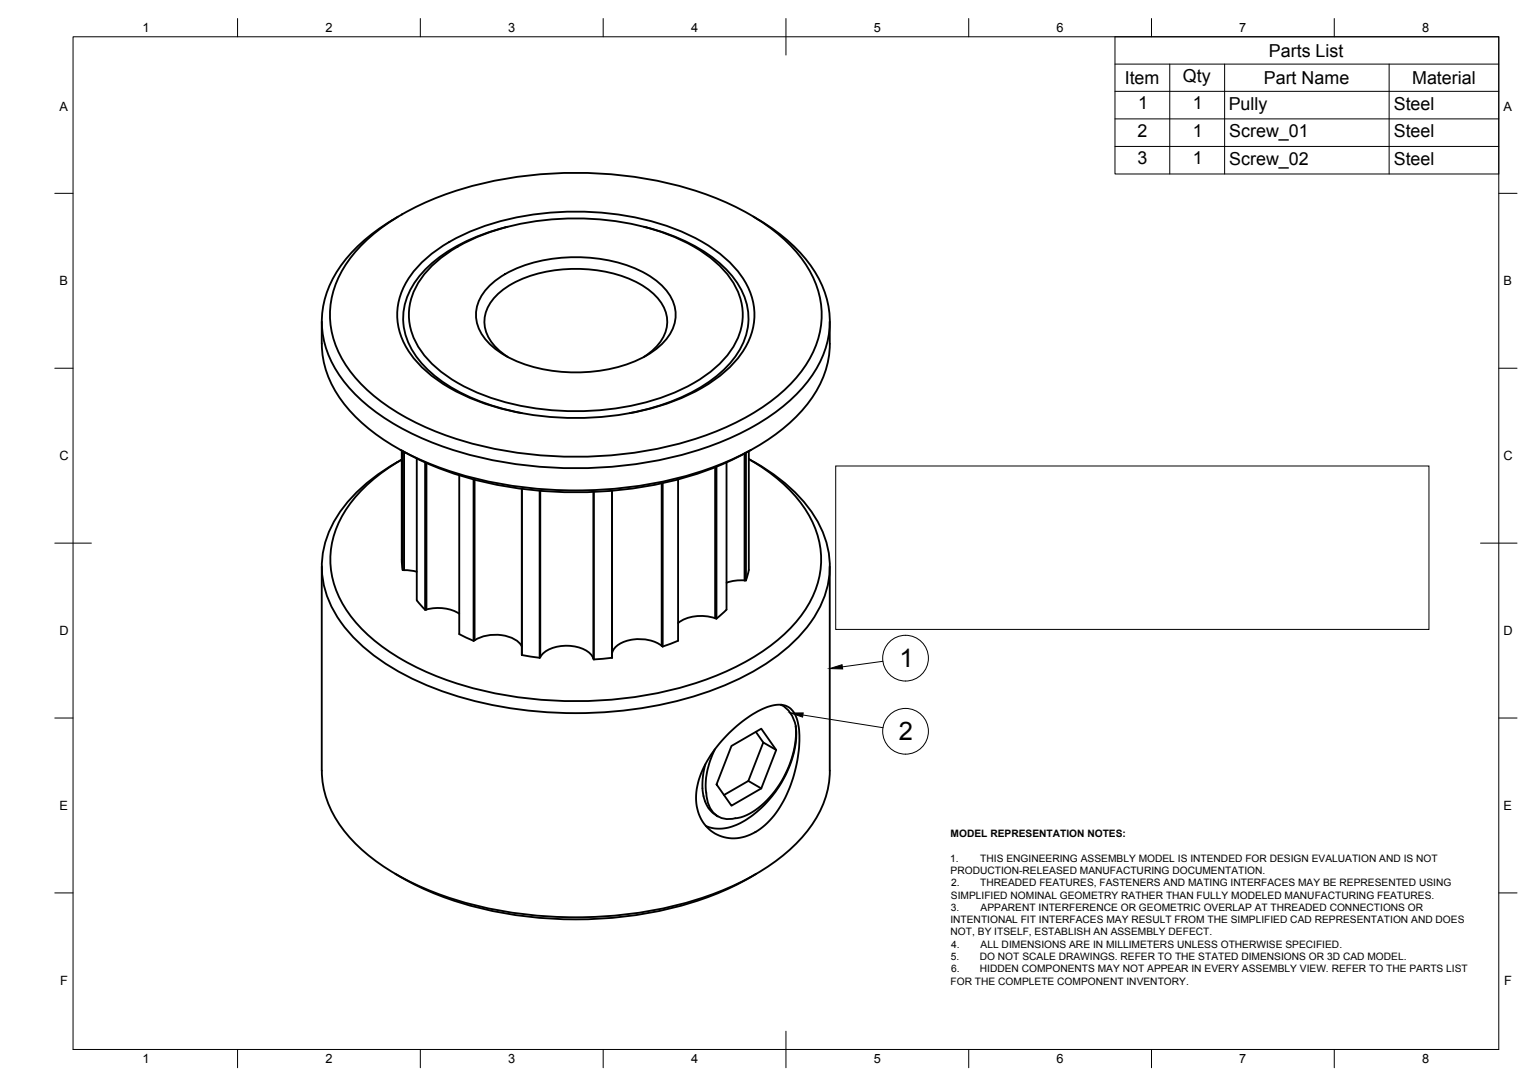
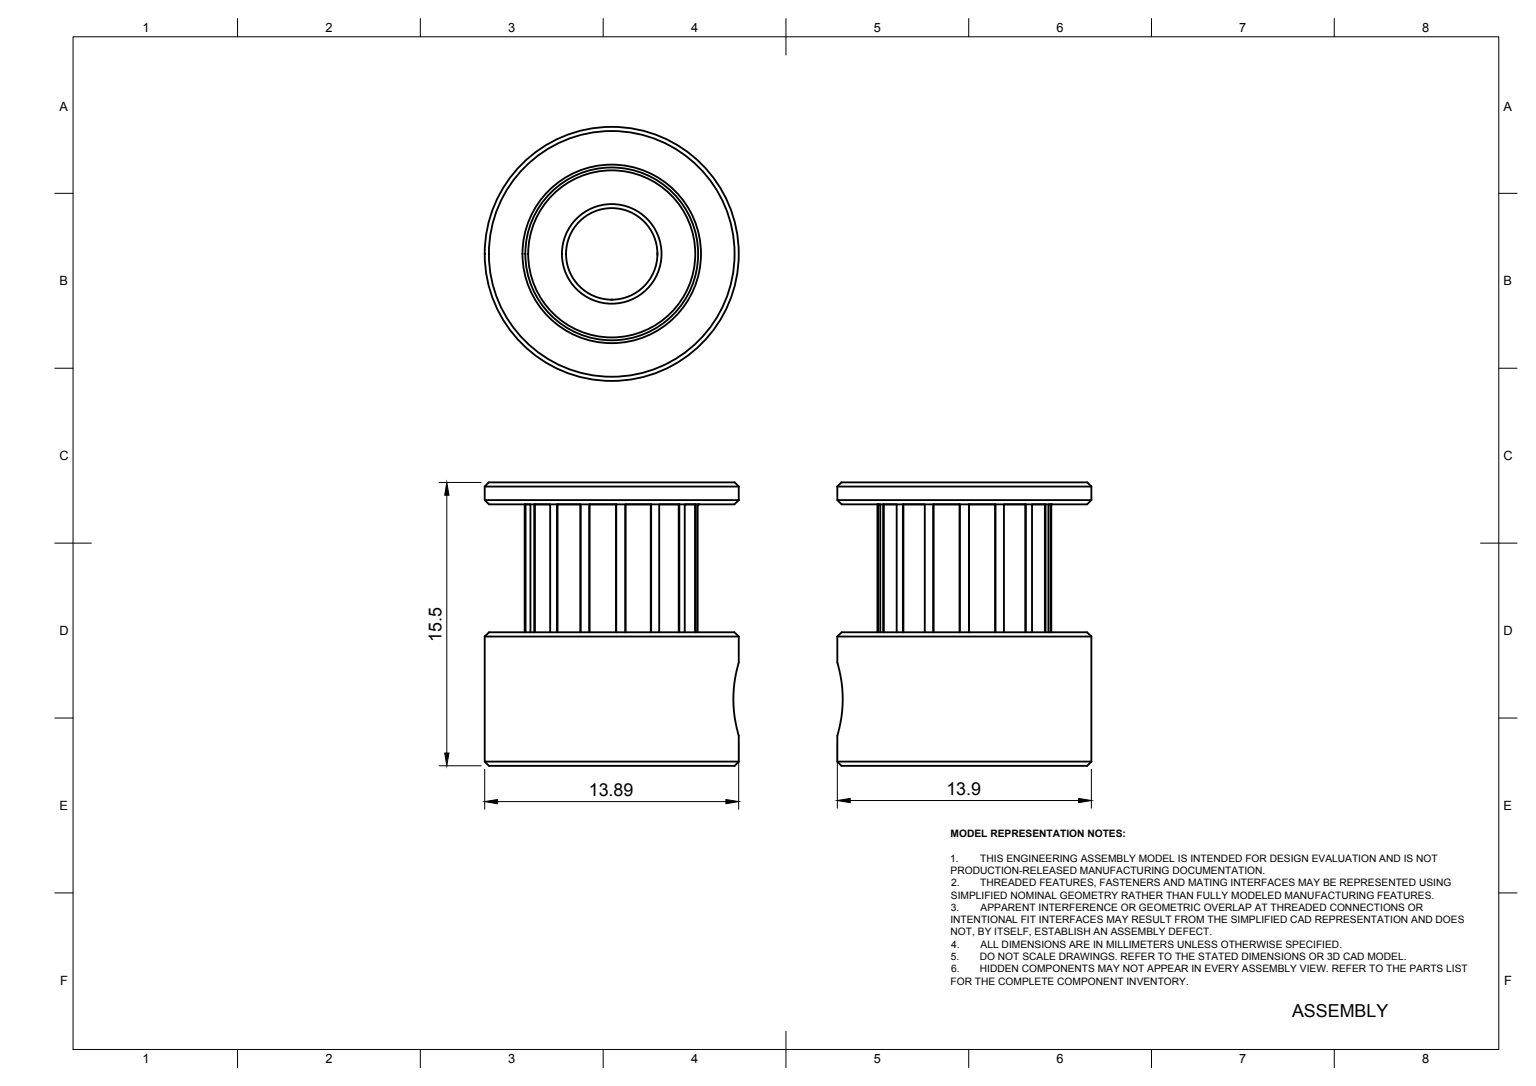
ISO-10303-21;
HEADER;
/* Generated by software containing ST-Developer
 * from STEP Tools, Inc. (www.steptools.com) 
 */

FILE_DESCRIPTION(
/* description */ (''),
/* implementation_level */ '2;1');

FILE_NAME(
/* name */ 'BR-253',
/* time_stamp */ '2026-10-05T21:25:27-07:00',
/* author */ (''),
/* organization */ (''),
/* preprocessor_version */ 'ST-DEVELOPER v20.2',
/* originating_system */ 'Autodesk Translation Framework v15.15.0.0',
/* authorisation */ '');

FILE_SCHEMA (('AUTOMOTIVE_DESIGN { 1 0 10303 214 3 1 1 }'));
ENDSEC;

DATA;
#10=MECHANICAL_DESIGN_GEOMETRIC_PRESENTATION_REPRESENTATION('',(#33,#34,
#35),#12118);
#11=ITEM_DEFINED_TRANSFORMATION($,$,#2444,#2723);
#12=ITEM_DEFINED_TRANSFORMATION($,$,#2667,#2724);
#13=ITEM_DEFINED_TRANSFORMATION($,$,#2695,#2725);
#14=(
REPRESENTATION_RELATIONSHIP($,$,#12135,#12134)
REPRESENTATION_RELATIONSHIP_WITH_TRANSFORMATION(#11)
SHAPE_REPRESENTATION_RELATIONSHIP()
);
#15=(
REPRESENTATION_RELATIONSHIP($,$,#12136,#12134)
REPRESENTATION_RELATIONSHIP_WITH_TRANSFORMATION(#12)
SHAPE_REPRESENTATION_RELATIONSHIP()
);
#16=(
REPRESENTATION_RELATIONSHIP($,$,#12137,#12134)
REPRESENTATION_RELATIONSHIP_WITH_TRANSFORMATION(#13)
SHAPE_REPRESENTATION_RELATIONSHIP()
);
#17=CONTEXT_DEPENDENT_SHAPE_REPRESENTATION(#14,#12131);
#18=CONTEXT_DEPENDENT_SHAPE_REPRESENTATION(#15,#12132);
#19=CONTEXT_DEPENDENT_SHAPE_REPRESENTATION(#16,#12133);
#20=NEXT_ASSEMBLY_USAGE_OCCURRENCE('Pully:1','Pully:1','Pully:1',#12139,
#12140,'Pully:1');
#21=NEXT_ASSEMBLY_USAGE_OCCURRENCE('Screw_01:1','Screw_01:1',
'Screw_01:1',#12139,#12141,'Screw_01:1');
#22=NEXT_ASSEMBLY_USAGE_OCCURRENCE('Screw_02:1','Screw_02:1',
'Screw_02:1',#12139,#12142,'Screw_02:1');
#23=B_SPLINE_SURFACE_WITH_KNOTS('',3,3,((#7351,#7352,#7353,#7354,#7355,
#7356,#7357,#7358,#7359,#7360,#7361,#7362,#7363,#7364,#7365,#7366,#7367,
#7368,#7369,#7370,#7371,#7372,#7373,#7374,#7375,#7376,#7377,#7378,#7379,
#7380,#7381,#7382,#7383,#7384,#7385,#7386,#7387,#7388,#7389,#7390,#7391,
#7392),(#7393,#7394,#7395,#7396,#7397,#7398,#7399,#7400,#7401,#7402,#7403,
#7404,#7405,#7406,#7407,#7408,#7409,#7410,#7411,#7412,#7413,#7414,#7415,
#7416,#7417,#7418,#7419,#7420,#7421,#7422,#7423,#7424,#7425,#7426,#7427,
#7428,#7429,#7430,#7431,#7432,#7433,#7434),(#7435,#7436,#7437,#7438,#7439,
#7440,#7441,#7442,#7443,#7444,#7445,#7446,#7447,#7448,#7449,#7450,#7451,
#7452,#7453,#7454,#7455,#7456,#7457,#7458,#7459,#7460,#7461,#7462,#7463,
#7464,#7465,#7466,#7467,#7468,#7469,#7470,#7471,#7472,#7473,#7474,#7475,
#7476),(#7477,#7478,#7479,#7480,#7481,#7482,#7483,#7484,#7485,#7486,#7487,
#7488,#7489,#7490,#7491,#7492,#7493,#7494,#7495,#7496,#7497,#7498,#7499,
#7500,#7501,#7502,#7503,#7504,#7505,#7506,#7507,#7508,#7509,#7510,#7511,
#7512,#7513,#7514,#7515,#7516,#7517,#7518)),.UNSPECIFIED.,.F.,.F.,.F.,(4,
4),(4,1,1,1,1,1,1,1,1,1,1,1,1,1,1,1,1,1,1,1,1,1,1,1,1,1,1,1,1,1,1,1,1,1,
1,1,1,1,1,4),(-0.000255169100126038,0.0463066876673496),(8.31044341387851,
9.3071677964662,10.3037486701926,11.300329543919,12.2969104176454,13.2934912913718,
14.2900721650982,15.2866530388247,16.2832339125511,17.2798147862775,18.2763956600039,
19.2729765337303,20.2695574074567,21.2661382811831,22.2627191549095,23.2593000286359,
24.2558809023623,25.2524617760888,26.2490426498152,27.2456235235416,28.242204397268,
29.2387852709944,30.2353661447208,31.2319470184472,32.2285278921736,33.2251087659,
34.2216896396264,35.2182705133528,36.2148513870793,37.2114322608057,38.2080131345321,
39.2045940082585,40.2011748819849,41.1977557557113,42.1943366294377,43.1909175031641,
44.1874983768905,45.1840792506169,46.1806601243433,47.1772409980698),
 .UNSPECIFIED.);
#24=B_SPLINE_SURFACE_WITH_KNOTS('',3,3,((#7695,#7696,#7697,#7698,#7699,
#7700,#7701,#7702,#7703,#7704,#7705,#7706,#7707,#7708,#7709,#7710,#7711,
#7712,#7713,#7714,#7715,#7716,#7717,#7718,#7719,#7720,#7721,#7722,#7723,
#7724,#7725,#7726,#7727,#7728,#7729,#7730,#7731,#7732,#7733,#7734,#7735,
#7736),(#7737,#7738,#7739,#7740,#7741,#7742,#7743,#7744,#7745,#7746,#7747,
#7748,#7749,#7750,#7751,#7752,#7753,#7754,#7755,#7756,#7757,#7758,#7759,
#7760,#7761,#7762,#7763,#7764,#7765,#7766,#7767,#7768,#7769,#7770,#7771,
#7772,#7773,#7774,#7775,#7776,#7777,#7778),(#7779,#7780,#7781,#7782,#7783,
#7784,#7785,#7786,#7787,#7788,#7789,#7790,#7791,#7792,#7793,#7794,#7795,
#7796,#7797,#7798,#7799,#7800,#7801,#7802,#7803,#7804,#7805,#7806,#7807,
#7808,#7809,#7810,#7811,#7812,#7813,#7814,#7815,#7816,#7817,#7818,#7819,
#7820),(#7821,#7822,#7823,#7824,#7825,#7826,#7827,#7828,#7829,#7830,#7831,
#7832,#7833,#7834,#7835,#7836,#7837,#7838,#7839,#7840,#7841,#7842,#7843,
#7844,#7845,#7846,#7847,#7848,#7849,#7850,#7851,#7852,#7853,#7854,#7855,
#7856,#7857,#7858,#7859,#7860,#7861,#7862)),.UNSPECIFIED.,.F.,.F.,.F.,(4,
4),(4,1,1,1,1,1,1,1,1,1,1,1,1,1,1,1,1,1,1,1,1,1,1,1,1,1,1,1,1,1,1,1,1,1,
1,1,1,1,1,4),(-0.000278939256451679,0.0463345324070479),(11.6151018031581,
12.6120023928371,13.6085832665635,14.6051641402899,15.6017450140163,16.5983258877427,
17.5949067614691,18.5914876351955,19.5880685089219,20.5846493826483,21.5812302563748,
22.5778111301012,23.5743920038276,24.570972877554,25.5675537512804,26.5641346250068,
27.5607154987332,28.5572963724596,29.553877246186,30.5504581199124,31.5470389936388,
32.5436198673653,33.5402007410917,34.5367816148181,35.5333624885445,36.5299433622709,
37.5265242359973,38.5231051097237,39.5196859834501,40.5162668571765,41.5128477309029,
42.5094286046293,43.5060094783558,44.5025903520822,45.4991712258086,46.495752099535,
47.4923329732614,48.4889138469878,49.4854947207142,50.4820755944406),
 .UNSPECIFIED.);
#25=B_SPLINE_SURFACE_WITH_KNOTS('',3,3,((#11379,#11380,#11381,#11382,#11383,
#11384,#11385,#11386,#11387,#11388,#11389,#11390,#11391,#11392,#11393,#11394,
#11395,#11396,#11397,#11398,#11399,#11400,#11401,#11402,#11403,#11404,#11405,
#11406,#11407,#11408,#11409,#11410,#11411,#11412,#11413,#11414,#11415,#11416,
#11417,#11418,#11419,#11420),(#11421,#11422,#11423,#11424,#11425,#11426,
#11427,#11428,#11429,#11430,#11431,#11432,#11433,#11434,#11435,#11436,#11437,
#11438,#11439,#11440,#11441,#11442,#11443,#11444,#11445,#11446,#11447,#11448,
#11449,#11450,#11451,#11452,#11453,#11454,#11455,#11456,#11457,#11458,#11459,
#11460,#11461,#11462),(#11463,#11464,#11465,#11466,#11467,#11468,#11469,
#11470,#11471,#11472,#11473,#11474,#11475,#11476,#11477,#11478,#11479,#11480,
#11481,#11482,#11483,#11484,#11485,#11486,#11487,#11488,#11489,#11490,#11491,
#11492,#11493,#11494,#11495,#11496,#11497,#11498,#11499,#11500,#11501,#11502,
#11503,#11504),(#11505,#11506,#11507,#11508,#11509,#11510,#11511,#11512,
#11513,#11514,#11515,#11516,#11517,#11518,#11519,#11520,#11521,#11522,#11523,
#11524,#11525,#11526,#11527,#11528,#11529,#11530,#11531,#11532,#11533,#11534,
#11535,#11536,#11537,#11538,#11539,#11540,#11541,#11542,#11543,#11544,#11545,
#11546)),.UNSPECIFIED.,.F.,.F.,.F.,(4,4),(4,1,1,1,1,1,1,1,1,1,1,1,1,1,1,
1,1,1,1,1,1,1,1,1,1,1,1,1,1,1,1,1,1,1,1,1,1,1,1,4),(-0.000255169100126093,
0.0463066876673497),(8.31044341387851,9.3071677964662,10.3037486701926,
11.300329543919,12.2969104176454,13.2934912913718,14.2900721650982,15.2866530388247,
16.2832339125511,17.2798147862775,18.2763956600039,19.2729765337303,20.2695574074567,
21.2661382811831,22.2627191549095,23.2593000286359,24.2558809023623,25.2524617760888,
26.2490426498152,27.2456235235416,28.242204397268,29.2387852709944,30.2353661447208,
31.2319470184472,32.2285278921736,33.2251087659,34.2216896396264,35.2182705133528,
36.2148513870793,37.2114322608057,38.2080131345321,39.2045940082585,40.2011748819849,
41.1977557557113,42.1943366294377,43.1909175031641,44.1874983768905,45.1840792506169,
46.1806601243433,47.1772409980698),.UNSPECIFIED.);
#26=B_SPLINE_SURFACE_WITH_KNOTS('',3,3,((#11723,#11724,#11725,#11726,#11727,
#11728,#11729,#11730,#11731,#11732,#11733,#11734,#11735,#11736,#11737,#11738,
#11739,#11740,#11741,#11742,#11743,#11744,#11745,#11746,#11747,#11748,#11749,
#11750,#11751,#11752,#11753,#11754,#11755,#11756,#11757,#11758,#11759,#11760,
#11761,#11762,#11763,#11764),(#11765,#11766,#11767,#11768,#11769,#11770,
#11771,#11772,#11773,#11774,#11775,#11776,#11777,#11778,#11779,#11780,#11781,
#11782,#11783,#11784,#11785,#11786,#11787,#11788,#11789,#11790,#11791,#11792,
#11793,#11794,#11795,#11796,#11797,#11798,#11799,#11800,#11801,#11802,#11803,
#11804,#11805,#11806),(#11807,#11808,#11809,#11810,#11811,#11812,#11813,
#11814,#11815,#11816,#11817,#11818,#11819,#11820,#11821,#11822,#11823,#11824,
#11825,#11826,#11827,#11828,#11829,#11830,#11831,#11832,#11833,#11834,#11835,
#11836,#11837,#11838,#11839,#11840,#11841,#11842,#11843,#11844,#11845,#11846,
#11847,#11848),(#11849,#11850,#11851,#11852,#11853,#11854,#11855,#11856,
#11857,#11858,#11859,#11860,#11861,#11862,#11863,#11864,#11865,#11866,#11867,
#11868,#11869,#11870,#11871,#11872,#11873,#11874,#11875,#11876,#11877,#11878,
#11879,#11880,#11881,#11882,#11883,#11884,#11885,#11886,#11887,#11888,#11889,
#11890)),.UNSPECIFIED.,.F.,.F.,.F.,(4,4),(4,1,1,1,1,1,1,1,1,1,1,1,1,1,1,
1,1,1,1,1,1,1,1,1,1,1,1,1,1,1,1,1,1,1,1,1,1,1,1,4),(-0.000278939256451637,
0.046334532407048),(11.6151018031581,12.6120023928371,13.6085832665635,
14.6051641402899,15.6017450140163,16.5983258877427,17.5949067614691,18.5914876351955,
19.5880685089219,20.5846493826483,21.5812302563748,22.5778111301012,23.5743920038276,
24.570972877554,25.5675537512804,26.5641346250068,27.5607154987332,28.5572963724596,
29.553877246186,30.5504581199124,31.5470389936388,32.5436198673653,33.5402007410917,
34.5367816148181,35.5333624885445,36.5299433622709,37.5265242359973,38.5231051097237,
39.5196859834501,40.5162668571765,41.5128477309029,42.5094286046293,43.5060094783558,
44.5025903520822,45.4991712258086,46.495752099535,47.4923329732614,48.4889138469878,
49.4854947207142,50.4820755944406),.UNSPECIFIED.);
#27=SHAPE_REPRESENTATION_RELATIONSHIP('SRR','None',#12135,#30);
#28=SHAPE_REPRESENTATION_RELATIONSHIP('SRR','None',#12136,#31);
#29=SHAPE_REPRESENTATION_RELATIONSHIP('SRR','None',#12137,#32);
#30=ADVANCED_BREP_SHAPE_REPRESENTATION('',(#36),#12115);
#31=ADVANCED_BREP_SHAPE_REPRESENTATION('',(#37),#12116);
#32=ADVANCED_BREP_SHAPE_REPRESENTATION('',(#38),#12117);
#33=STYLED_ITEM('',(#12159),#36);
#34=STYLED_ITEM('',(#12159),#37);
#35=STYLED_ITEM('',(#12159),#38);
#36=MANIFOLD_SOLID_BREP('Body1',#2406);
#37=MANIFOLD_SOLID_BREP('Body1',#2407);
#38=MANIFOLD_SOLID_BREP('Body1',#2408);
#39=CONICAL_SURFACE('',#2637,6.82923606324244,0.788206310939685);
#40=CONICAL_SURFACE('',#2641,6.83201065632366,0.782590015855212);
#41=CONICAL_SURFACE('',#2645,4.80296382139185,0.926815431707518);
#42=CONICAL_SURFACE('',#2647,4.64521779108966,0.920500215637548);
#43=CONICAL_SURFACE('',#2651,2.61128051468949,0.789543103695558);
#44=CONICAL_SURFACE('',#2652,2.61559010295572,0.781253223099339);
#45=CONICAL_SURFACE('',#2656,4.64520588040018,0.911866720012535);
#46=CONICAL_SURFACE('',#2658,4.80503122320831,0.931803832862888);
#47=CONICAL_SURFACE('',#2662,6.83593993841137,0.77406839497658);
#48=CONICAL_SURFACE('',#2666,6.82905809599587,0.796727931818318);
#49=FACE_BOUND('',#442,.T.);
#50=FACE_BOUND('',#444,.T.);
#51=FACE_BOUND('',#447,.T.);
#52=FACE_BOUND('',#450,.T.);
#53=FACE_BOUND('',#454,.T.);
#54=FACE_BOUND('',#458,.T.);
#55=FACE_BOUND('',#462,.T.);
#56=FACE_BOUND('',#483,.T.);
#57=FACE_BOUND('',#509,.T.);
#58=PLANE('',#2453);
#59=PLANE('',#2464);
#60=PLANE('',#2475);
#61=PLANE('',#2486);
#62=PLANE('',#2497);
#63=PLANE('',#2508);
#64=PLANE('',#2519);
#65=PLANE('',#2530);
#66=PLANE('',#2541);
#67=PLANE('',#2552);
#68=PLANE('',#2563);
#69=PLANE('',#2574);
#70=PLANE('',#2585);
#71=PLANE('',#2596);
#72=PLANE('',#2626);
#73=PLANE('',#2633);
#74=PLANE('',#2635);
#75=PLANE('',#2643);
#76=PLANE('',#2649);
#77=PLANE('',#2654);
#78=PLANE('',#2660);
#79=PLANE('',#2686);
#80=PLANE('',#2687);
#81=PLANE('',#2688);
#82=PLANE('',#2689);
#83=PLANE('',#2690);
#84=PLANE('',#2691);
#85=PLANE('',#2692);
#86=PLANE('',#2693);
#87=PLANE('',#2694);
#88=PLANE('',#2714);
#89=PLANE('',#2715);
#90=PLANE('',#2716);
#91=PLANE('',#2717);
#92=PLANE('',#2718);
#93=PLANE('',#2719);
#94=PLANE('',#2720);
#95=PLANE('',#2721);
#96=PLANE('',#2722);
#97=CIRCLE('',#2447,2.50080065552765);
#98=CIRCLE('',#2448,2.50080065552765);
#99=CIRCLE('',#2451,0.124032861755453);
#100=CIRCLE('',#2452,0.124032861755453);
#101=CIRCLE('',#2454,4.75930776765241);
#102=CIRCLE('',#2455,0.749041401963156);
#103=CIRCLE('',#2456,0.124032861755453);
#104=CIRCLE('',#2458,0.749041401963156);
#105=CIRCLE('',#2460,0.124032861755453);
#106=CIRCLE('',#2462,0.124032861755453);
#107=CIRCLE('',#2463,0.124032861755453);
#108=CIRCLE('',#2465,4.75930776765241);
#109=CIRCLE('',#2466,0.749041401963156);
#110=CIRCLE('',#2467,0.124032861755453);
#111=CIRCLE('',#2469,0.749041401963156);
#112=CIRCLE('',#2471,0.124032861755453);
#113=CIRCLE('',#2473,0.124032861755453);
#114=CIRCLE('',#2474,0.124032861755453);
#115=CIRCLE('',#2476,4.75930776765241);
#116=CIRCLE('',#2477,0.749041401963155);
#117=CIRCLE('',#2478,0.124032861755453);
#118=CIRCLE('',#2480,0.749041401963155);
#119=CIRCLE('',#2482,0.124032861755453);
#120=CIRCLE('',#2484,0.124032861755453);
#121=CIRCLE('',#2485,0.124032861755453);
#122=CIRCLE('',#2487,4.75930776765241);
#123=CIRCLE('',#2488,0.749041401963156);
#124=CIRCLE('',#2489,0.124032861755453);
#125=CIRCLE('',#2491,0.749041401963156);
#126=CIRCLE('',#2493,0.124032861755453);
#127=CIRCLE('',#2495,0.124032861755453);
#128=CIRCLE('',#2496,0.124032861755453);
#129=CIRCLE('',#2498,4.75930776765241);
#130=CIRCLE('',#2499,0.749041401963155);
#131=CIRCLE('',#2500,0.124032861755453);
#132=CIRCLE('',#2502,0.749041401963155);
#133=CIRCLE('',#2504,0.124032861755453);
#134=CIRCLE('',#2506,0.124032861755453);
#135=CIRCLE('',#2507,0.124032861755453);
#136=CIRCLE('',#2509,4.75930776765241);
#137=CIRCLE('',#2510,0.749041401963156);
#138=CIRCLE('',#2511,0.124032861755453);
#139=CIRCLE('',#2513,0.749041401963156);
#140=CIRCLE('',#2515,0.124032861755453);
#141=CIRCLE('',#2517,0.124032861755453);
#142=CIRCLE('',#2518,0.124032861755453);
#143=CIRCLE('',#2520,4.75930776765241);
#144=CIRCLE('',#2521,0.749041401963155);
#145=CIRCLE('',#2522,0.124032861755453);
#146=CIRCLE('',#2524,0.749041401963155);
#147=CIRCLE('',#2526,0.124032861755453);
#148=CIRCLE('',#2528,0.124032861755453);
#149=CIRCLE('',#2529,0.124032861755453);
#150=CIRCLE('',#2531,4.75930776765241);
#151=CIRCLE('',#2532,0.749041401963156);
#152=CIRCLE('',#2533,0.124032861755453);
#153=CIRCLE('',#2535,0.749041401963156);
#154=CIRCLE('',#2537,0.124032861755453);
#155=CIRCLE('',#2539,0.124032861755453);
#156=CIRCLE('',#2540,0.124032861755453);
#157=CIRCLE('',#2542,4.75930776765241);
#158=CIRCLE('',#2543,0.749041401963155);
#159=CIRCLE('',#2544,0.124032861755453);
#160=CIRCLE('',#2546,0.749041401963155);
#161=CIRCLE('',#2548,0.124032861755453);
#162=CIRCLE('',#2550,0.124032861755453);
#163=CIRCLE('',#2551,0.124032861755453);
#164=CIRCLE('',#2553,4.75930776765241);
#165=CIRCLE('',#2554,0.749041401963156);
#166=CIRCLE('',#2555,0.124032861755453);
#167=CIRCLE('',#2557,0.749041401963156);
#168=CIRCLE('',#2559,0.124032861755453);
#169=CIRCLE('',#2561,0.124032861755453);
#170=CIRCLE('',#2562,0.124032861755453);
#171=CIRCLE('',#2564,4.75930776765241);
#172=CIRCLE('',#2565,0.749041401963156);
#173=CIRCLE('',#2566,0.124032861755453);
#174=CIRCLE('',#2568,0.749041401963156);
#175=CIRCLE('',#2570,0.124032861755453);
#176=CIRCLE('',#2572,0.124032861755453);
#177=CIRCLE('',#2573,0.124032861755453);
#178=CIRCLE('',#2575,4.75930776765241);
#179=CIRCLE('',#2576,0.749041401963155);
#180=CIRCLE('',#2577,0.124032861755453);
#181=CIRCLE('',#2579,0.749041401963155);
#182=CIRCLE('',#2581,0.124032861755453);
#183=CIRCLE('',#2583,0.124032861755453);
#184=CIRCLE('',#2584,0.124032861755453);
#185=CIRCLE('',#2586,4.75930776765241);
#186=CIRCLE('',#2587,0.749041401963156);
#187=CIRCLE('',#2588,0.124032861755453);
#188=CIRCLE('',#2590,0.749041401963156);
#189=CIRCLE('',#2592,0.124032861755453);
#190=CIRCLE('',#2594,0.124032861755453);
#191=CIRCLE('',#2595,0.124032861755453);
#192=CIRCLE('',#2597,4.75930776765241);
#193=CIRCLE('',#2598,0.749041401963155);
#194=CIRCLE('',#2599,0.124032861755453);
#195=CIRCLE('',#2601,0.749041401963155);
#196=CIRCLE('',#2603,0.124032861755453);
#197=CIRCLE('',#2605,4.75930776765241);
#198=CIRCLE('',#2606,4.75930776765241);
#199=CIRCLE('',#2607,4.75930776765241);
#200=CIRCLE('',#2608,4.75930776765241);
#201=CIRCLE('',#2609,4.75930776765241);
#202=CIRCLE('',#2610,4.75930776765241);
#203=CIRCLE('',#2611,4.75930776765241);
#204=CIRCLE('',#2612,4.75930776765241);
#205=CIRCLE('',#2613,4.75930776765241);
#206=CIRCLE('',#2614,4.75930776765241);
#207=CIRCLE('',#2615,4.75930776765241);
#208=CIRCLE('',#2616,4.75930776765241);
#209=CIRCLE('',#2617,4.75930776765241);
#210=CIRCLE('',#2618,4.75930776765241);
#211=CIRCLE('',#2619,4.75930776765241);
#212=CIRCLE('',#2620,4.75930776765241);
#213=CIRCLE('',#2621,4.75930776765241);
#214=CIRCLE('',#2622,4.75930776765241);
#215=CIRCLE('',#2624,0.124032861755453);
#216=CIRCLE('',#2625,0.124032861755453);
#217=CIRCLE('',#2627,0.749041401963155);
#218=CIRCLE('',#2628,0.124032861755453);
#219=CIRCLE('',#2630,0.749041401963155);
#220=CIRCLE('',#2632,0.124032861755453);
#221=CIRCLE('',#2634,6.71146155382814);
#222=CIRCLE('',#2636,6.71146155382814);
#223=CIRCLE('',#2638,6.94701057265674);
#224=CIRCLE('',#2640,6.94701057265674);
#225=CIRCLE('',#2642,6.71701073999059);
#226=CIRCLE('',#2644,4.88235460250674);
#227=CIRCLE('',#2646,4.72357304027696);
#228=CIRCLE('',#2648,4.56686254190236);
#229=CIRCLE('',#2650,2.72176037385134);
#230=CIRCLE('',#2653,2.7303795503838);
#231=CIRCLE('',#2655,4.56694754124435);
#232=CIRCLE('',#2657,4.72346421955602);
#233=CIRCLE('',#2659,4.8865982268606);
#234=CIRCLE('',#2661,6.72522523865914);
#235=CIRCLE('',#2663,6.94665463816359);
#236=CIRCLE('',#2665,6.94665463816359);
#237=CIRCLE('',#2669,1.5555);
#238=CIRCLE('',#2676,1.954);
#239=CIRCLE('',#2683,1.954);
#240=CIRCLE('',#2685,1.5555);
#241=CIRCLE('',#2697,1.5555);
#242=CIRCLE('',#2704,1.954);
#243=CIRCLE('',#2711,1.954);
#244=CIRCLE('',#2713,1.5555);
#245=FACE_OUTER_BOUND('',#377,.T.);
#246=FACE_OUTER_BOUND('',#378,.T.);
#247=FACE_OUTER_BOUND('',#379,.T.);
#248=FACE_OUTER_BOUND('',#380,.T.);
#249=FACE_OUTER_BOUND('',#381,.T.);
#250=FACE_OUTER_BOUND('',#382,.T.);
#251=FACE_OUTER_BOUND('',#383,.T.);
#252=FACE_OUTER_BOUND('',#384,.T.);
#253=FACE_OUTER_BOUND('',#385,.T.);
#254=FACE_OUTER_BOUND('',#386,.T.);
#255=FACE_OUTER_BOUND('',#387,.T.);
#256=FACE_OUTER_BOUND('',#388,.T.);
#257=FACE_OUTER_BOUND('',#389,.T.);
#258=FACE_OUTER_BOUND('',#390,.T.);
#259=FACE_OUTER_BOUND('',#391,.T.);
#260=FACE_OUTER_BOUND('',#392,.T.);
#261=FACE_OUTER_BOUND('',#393,.T.);
#262=FACE_OUTER_BOUND('',#394,.T.);
#263=FACE_OUTER_BOUND('',#395,.T.);
#264=FACE_OUTER_BOUND('',#396,.T.);
#265=FACE_OUTER_BOUND('',#397,.T.);
#266=FACE_OUTER_BOUND('',#398,.T.);
#267=FACE_OUTER_BOUND('',#399,.T.);
#268=FACE_OUTER_BOUND('',#400,.T.);
#269=FACE_OUTER_BOUND('',#401,.T.);
#270=FACE_OUTER_BOUND('',#402,.T.);
#271=FACE_OUTER_BOUND('',#403,.T.);
#272=FACE_OUTER_BOUND('',#404,.T.);
#273=FACE_OUTER_BOUND('',#405,.T.);
#274=FACE_OUTER_BOUND('',#406,.T.);
#275=FACE_OUTER_BOUND('',#407,.T.);
#276=FACE_OUTER_BOUND('',#408,.T.);
#277=FACE_OUTER_BOUND('',#409,.T.);
#278=FACE_OUTER_BOUND('',#410,.T.);
#279=FACE_OUTER_BOUND('',#411,.T.);
#280=FACE_OUTER_BOUND('',#412,.T.);
#281=FACE_OUTER_BOUND('',#413,.T.);
#282=FACE_OUTER_BOUND('',#414,.T.);
#283=FACE_OUTER_BOUND('',#415,.T.);
#284=FACE_OUTER_BOUND('',#416,.T.);
#285=FACE_OUTER_BOUND('',#417,.T.);
#286=FACE_OUTER_BOUND('',#418,.T.);
#287=FACE_OUTER_BOUND('',#419,.T.);
#288=FACE_OUTER_BOUND('',#420,.T.);
#289=FACE_OUTER_BOUND('',#421,.T.);
#290=FACE_OUTER_BOUND('',#422,.T.);
#291=FACE_OUTER_BOUND('',#423,.T.);
#292=FACE_OUTER_BOUND('',#424,.T.);
#293=FACE_OUTER_BOUND('',#425,.T.);
#294=FACE_OUTER_BOUND('',#426,.T.);
#295=FACE_OUTER_BOUND('',#427,.T.);
#296=FACE_OUTER_BOUND('',#428,.T.);
#297=FACE_OUTER_BOUND('',#429,.T.);
#298=FACE_OUTER_BOUND('',#430,.T.);
#299=FACE_OUTER_BOUND('',#431,.T.);
#300=FACE_OUTER_BOUND('',#432,.T.);
#301=FACE_OUTER_BOUND('',#433,.T.);
#302=FACE_OUTER_BOUND('',#434,.T.);
#303=FACE_OUTER_BOUND('',#435,.T.);
#304=FACE_OUTER_BOUND('',#436,.T.);
#305=FACE_OUTER_BOUND('',#437,.T.);
#306=FACE_OUTER_BOUND('',#438,.T.);
#307=FACE_OUTER_BOUND('',#439,.T.);
#308=FACE_OUTER_BOUND('',#440,.T.);
#309=FACE_OUTER_BOUND('',#441,.T.);
#310=FACE_OUTER_BOUND('',#443,.T.);
#311=FACE_OUTER_BOUND('',#445,.T.);
#312=FACE_OUTER_BOUND('',#446,.T.);
#313=FACE_OUTER_BOUND('',#448,.T.);
#314=FACE_OUTER_BOUND('',#449,.T.);
#315=FACE_OUTER_BOUND('',#451,.T.);
#316=FACE_OUTER_BOUND('',#452,.T.);
#317=FACE_OUTER_BOUND('',#453,.T.);
#318=FACE_OUTER_BOUND('',#455,.T.);
#319=FACE_OUTER_BOUND('',#456,.T.);
#320=FACE_OUTER_BOUND('',#457,.T.);
#321=FACE_OUTER_BOUND('',#459,.T.);
#322=FACE_OUTER_BOUND('',#460,.T.);
#323=FACE_OUTER_BOUND('',#461,.T.);
#324=FACE_OUTER_BOUND('',#463,.T.);
#325=FACE_OUTER_BOUND('',#464,.T.);
#326=FACE_OUTER_BOUND('',#465,.T.);
#327=FACE_OUTER_BOUND('',#466,.T.);
#328=FACE_OUTER_BOUND('',#467,.T.);
#329=FACE_OUTER_BOUND('',#468,.T.);
#330=FACE_OUTER_BOUND('',#469,.T.);
#331=FACE_OUTER_BOUND('',#470,.T.);
#332=FACE_OUTER_BOUND('',#471,.T.);
#333=FACE_OUTER_BOUND('',#472,.T.);
#334=FACE_OUTER_BOUND('',#473,.T.);
#335=FACE_OUTER_BOUND('',#474,.T.);
#336=FACE_OUTER_BOUND('',#475,.T.);
#337=FACE_OUTER_BOUND('',#476,.T.);
#338=FACE_OUTER_BOUND('',#477,.T.);
#339=FACE_OUTER_BOUND('',#478,.T.);
#340=FACE_OUTER_BOUND('',#479,.T.);
#341=FACE_OUTER_BOUND('',#480,.T.);
#342=FACE_OUTER_BOUND('',#481,.T.);
#343=FACE_OUTER_BOUND('',#482,.T.);
#344=FACE_OUTER_BOUND('',#484,.T.);
#345=FACE_OUTER_BOUND('',#485,.T.);
#346=FACE_OUTER_BOUND('',#486,.T.);
#347=FACE_OUTER_BOUND('',#487,.T.);
#348=FACE_OUTER_BOUND('',#488,.T.);
#349=FACE_OUTER_BOUND('',#489,.T.);
#350=FACE_OUTER_BOUND('',#490,.T.);
#351=FACE_OUTER_BOUND('',#491,.T.);
#352=FACE_OUTER_BOUND('',#492,.T.);
#353=FACE_OUTER_BOUND('',#493,.T.);
#354=FACE_OUTER_BOUND('',#494,.T.);
#355=FACE_OUTER_BOUND('',#495,.T.);
#356=FACE_OUTER_BOUND('',#496,.T.);
#357=FACE_OUTER_BOUND('',#497,.T.);
#358=FACE_OUTER_BOUND('',#498,.T.);
#359=FACE_OUTER_BOUND('',#499,.T.);
#360=FACE_OUTER_BOUND('',#500,.T.);
#361=FACE_OUTER_BOUND('',#501,.T.);
#362=FACE_OUTER_BOUND('',#502,.T.);
#363=FACE_OUTER_BOUND('',#503,.T.);
#364=FACE_OUTER_BOUND('',#504,.T.);
#365=FACE_OUTER_BOUND('',#505,.T.);
#366=FACE_OUTER_BOUND('',#506,.T.);
#367=FACE_OUTER_BOUND('',#507,.T.);
#368=FACE_OUTER_BOUND('',#508,.T.);
#369=FACE_OUTER_BOUND('',#510,.T.);
#370=FACE_OUTER_BOUND('',#511,.T.);
#371=FACE_OUTER_BOUND('',#512,.T.);
#372=FACE_OUTER_BOUND('',#513,.T.);
#373=FACE_OUTER_BOUND('',#514,.T.);
#374=FACE_OUTER_BOUND('',#515,.T.);
#375=FACE_OUTER_BOUND('',#516,.T.);
#376=FACE_OUTER_BOUND('',#517,.T.);
#377=EDGE_LOOP('',(#1471,#1472,#1473,#1474,#1475,#1476,#1477));
#378=EDGE_LOOP('',(#1478,#1479,#1480,#1481,#1482,#1483,#1484,#1485,#1486,
#1487,#1488,#1489));
#379=EDGE_LOOP('',(#1490,#1491,#1492,#1493,#1494,#1495,#1496,#1497,#1498,
#1499));
#380=EDGE_LOOP('',(#1500,#1501,#1502,#1503));
#381=EDGE_LOOP('',(#1504,#1505,#1506,#1507));
#382=EDGE_LOOP('',(#1508,#1509,#1510,#1511));
#383=EDGE_LOOP('',(#1512,#1513,#1514,#1515));
#384=EDGE_LOOP('',(#1516,#1517,#1518,#1519));
#385=EDGE_LOOP('',(#1520,#1521,#1522,#1523));
#386=EDGE_LOOP('',(#1524,#1525,#1526,#1527));
#387=EDGE_LOOP('',(#1528,#1529,#1530,#1531));
#388=EDGE_LOOP('',(#1532,#1533,#1534,#1535));
#389=EDGE_LOOP('',(#1536,#1537,#1538,#1539));
#390=EDGE_LOOP('',(#1540,#1541,#1542,#1543));
#391=EDGE_LOOP('',(#1544,#1545,#1546,#1547));
#392=EDGE_LOOP('',(#1548,#1549,#1550,#1551));
#393=EDGE_LOOP('',(#1552,#1553,#1554,#1555));
#394=EDGE_LOOP('',(#1556,#1557,#1558,#1559));
#395=EDGE_LOOP('',(#1560,#1561,#1562,#1563));
#396=EDGE_LOOP('',(#1564,#1565,#1566,#1567));
#397=EDGE_LOOP('',(#1568,#1569,#1570,#1571));
#398=EDGE_LOOP('',(#1572,#1573,#1574,#1575));
#399=EDGE_LOOP('',(#1576,#1577,#1578,#1579));
#400=EDGE_LOOP('',(#1580,#1581,#1582,#1583));
#401=EDGE_LOOP('',(#1584,#1585,#1586,#1587));
#402=EDGE_LOOP('',(#1588,#1589,#1590,#1591));
#403=EDGE_LOOP('',(#1592,#1593,#1594,#1595));
#404=EDGE_LOOP('',(#1596,#1597,#1598,#1599));
#405=EDGE_LOOP('',(#1600,#1601,#1602,#1603));
#406=EDGE_LOOP('',(#1604,#1605,#1606,#1607));
#407=EDGE_LOOP('',(#1608,#1609,#1610,#1611));
#408=EDGE_LOOP('',(#1612,#1613,#1614,#1615));
#409=EDGE_LOOP('',(#1616,#1617,#1618,#1619));
#410=EDGE_LOOP('',(#1620,#1621,#1622,#1623));
#411=EDGE_LOOP('',(#1624,#1625,#1626,#1627));
#412=EDGE_LOOP('',(#1628,#1629,#1630,#1631));
#413=EDGE_LOOP('',(#1632,#1633,#1634,#1635));
#414=EDGE_LOOP('',(#1636,#1637,#1638,#1639));
#415=EDGE_LOOP('',(#1640,#1641,#1642,#1643));
#416=EDGE_LOOP('',(#1644,#1645,#1646,#1647));
#417=EDGE_LOOP('',(#1648,#1649,#1650,#1651));
#418=EDGE_LOOP('',(#1652,#1653,#1654,#1655));
#419=EDGE_LOOP('',(#1656,#1657,#1658,#1659));
#420=EDGE_LOOP('',(#1660,#1661,#1662,#1663));
#421=EDGE_LOOP('',(#1664,#1665,#1666,#1667));
#422=EDGE_LOOP('',(#1668,#1669,#1670,#1671));
#423=EDGE_LOOP('',(#1672,#1673,#1674,#1675));
#424=EDGE_LOOP('',(#1676,#1677,#1678,#1679));
#425=EDGE_LOOP('',(#1680,#1681,#1682,#1683));
#426=EDGE_LOOP('',(#1684,#1685,#1686,#1687));
#427=EDGE_LOOP('',(#1688,#1689,#1690,#1691));
#428=EDGE_LOOP('',(#1692,#1693,#1694,#1695));
#429=EDGE_LOOP('',(#1696,#1697,#1698,#1699));
#430=EDGE_LOOP('',(#1700,#1701,#1702,#1703));
#431=EDGE_LOOP('',(#1704,#1705,#1706,#1707));
#432=EDGE_LOOP('',(#1708,#1709,#1710,#1711));
#433=EDGE_LOOP('',(#1712,#1713,#1714,#1715));
#434=EDGE_LOOP('',(#1716,#1717,#1718,#1719));
#435=EDGE_LOOP('',(#1720,#1721,#1722,#1723));
#436=EDGE_LOOP('',(#1724,#1725,#1726,#1727,#1728,#1729,#1730,#1731,#1732,
#1733,#1734,#1735,#1736,#1737,#1738,#1739,#1740,#1741,#1742,#1743,#1744,
#1745,#1746,#1747,#1748,#1749,#1750,#1751,#1752,#1753,#1754,#1755,#1756,
#1757,#1758,#1759,#1760,#1761,#1762,#1763,#1764,#1765,#1766,#1767,#1768,
#1769,#1770,#1771,#1772,#1773,#1774,#1775,#1776,#1777,#1778,#1779,#1780,
#1781,#1782,#1783,#1784,#1785,#1786,#1787));
#437=EDGE_LOOP('',(#1788,#1789,#1790,#1791));
#438=EDGE_LOOP('',(#1792,#1793,#1794,#1795,#1796));
#439=EDGE_LOOP('',(#1797,#1798,#1799,#1800));
#440=EDGE_LOOP('',(#1801,#1802,#1803,#1804));
#441=EDGE_LOOP('',(#1805));
#442=EDGE_LOOP('',(#1806));
#443=EDGE_LOOP('',(#1807));
#444=EDGE_LOOP('',(#1808,#1809,#1810,#1811,#1812,#1813,#1814,#1815,#1816,
#1817,#1818,#1819,#1820,#1821,#1822,#1823,#1824,#1825,#1826,#1827,#1828,
#1829,#1830,#1831,#1832,#1833,#1834,#1835,#1836,#1837,#1838,#1839,#1840,
#1841,#1842,#1843,#1844,#1845,#1846,#1847,#1848,#1849,#1850,#1851,#1852,
#1853,#1854,#1855,#1856,#1857,#1858,#1859,#1860,#1861,#1862,#1863,#1864,
#1865,#1866,#1867));
#445=EDGE_LOOP('',(#1868,#1869,#1870,#1871));
#446=EDGE_LOOP('',(#1872,#1873,#1874,#1875,#1876,#1877,#1878,#1879,#1880));
#447=EDGE_LOOP('',(#1881,#1882));
#448=EDGE_LOOP('',(#1883,#1884,#1885,#1886));
#449=EDGE_LOOP('',(#1887));
#450=EDGE_LOOP('',(#1888));
#451=EDGE_LOOP('',(#1889,#1890,#1891,#1892));
#452=EDGE_LOOP('',(#1893,#1894,#1895,#1896));
#453=EDGE_LOOP('',(#1897));
#454=EDGE_LOOP('',(#1898));
#455=EDGE_LOOP('',(#1899,#1900,#1901,#1902));
#456=EDGE_LOOP('',(#1903,#1904,#1905,#1906));
#457=EDGE_LOOP('',(#1907));
#458=EDGE_LOOP('',(#1908));
#459=EDGE_LOOP('',(#1909,#1910,#1911,#1912));
#460=EDGE_LOOP('',(#1913,#1914,#1915,#1916));
#461=EDGE_LOOP('',(#1917));
#462=EDGE_LOOP('',(#1918));
#463=EDGE_LOOP('',(#1919,#1920,#1921,#1922));
#464=EDGE_LOOP('',(#1923,#1924,#1925,#1926));
#465=EDGE_LOOP('',(#1927,#1928,#1929,#1930));
#466=EDGE_LOOP('',(#1931,#1932,#1933,#1934));
#467=EDGE_LOOP('',(#1935,#1936,#1937,#1938));
#468=EDGE_LOOP('',(#1939,#1940,#1941,#1942));
#469=EDGE_LOOP('',(#1943,#1944,#1945,#1946));
#470=EDGE_LOOP('',(#1947,#1948,#1949,#1950));
#471=EDGE_LOOP('',(#1951,#1952,#1953,#1954));
#472=EDGE_LOOP('',(#1955,#1956,#1957,#1958));
#473=EDGE_LOOP('',(#1959,#1960,#1961,#1962));
#474=EDGE_LOOP('',(#1963,#1964,#1965,#1966));
#475=EDGE_LOOP('',(#1967,#1968,#1969,#1970));
#476=EDGE_LOOP('',(#1971,#1972,#1973,#1974));
#477=EDGE_LOOP('',(#1975,#1976,#1977,#1978));
#478=EDGE_LOOP('',(#1979,#1980,#1981,#1982));
#479=EDGE_LOOP('',(#1983,#1984,#1985,#1986));
#480=EDGE_LOOP('',(#1987,#1988,#1989,#1990,#1991,#1992,#1993,#1994,#1995,
#1996,#1997,#1998,#1999,#2000,#2001,#2002));
#481=EDGE_LOOP('',(#2003,#2004,#2005,#2006,#2007,#2008,#2009,#2010,#2011,
#2012,#2013,#2014,#2015,#2016,#2017,#2018));
#482=EDGE_LOOP('',(#2019,#2020,#2021,#2022));
#483=EDGE_LOOP('',(#2023,#2024,#2025,#2026,#2027,#2028));
#484=EDGE_LOOP('',(#2029,#2030,#2031,#2032));
#485=EDGE_LOOP('',(#2033,#2034,#2035,#2036));
#486=EDGE_LOOP('',(#2037,#2038,#2039,#2040));
#487=EDGE_LOOP('',(#2041,#2042,#2043,#2044));
#488=EDGE_LOOP('',(#2045,#2046,#2047,#2048));
#489=EDGE_LOOP('',(#2049,#2050,#2051,#2052));
#490=EDGE_LOOP('',(#2053,#2054,#2055,#2056,#2057,#2058));
#491=EDGE_LOOP('',(#2059,#2060,#2061,#2062));
#492=EDGE_LOOP('',(#2063,#2064,#2065,#2066));
#493=EDGE_LOOP('',(#2067,#2068,#2069,#2070));
#494=EDGE_LOOP('',(#2071,#2072,#2073,#2074));
#495=EDGE_LOOP('',(#2075,#2076,#2077,#2078));
#496=EDGE_LOOP('',(#2079,#2080,#2081,#2082));
#497=EDGE_LOOP('',(#2083,#2084,#2085,#2086));
#498=EDGE_LOOP('',(#2087,#2088,#2089,#2090));
#499=EDGE_LOOP('',(#2091,#2092,#2093,#2094));
#500=EDGE_LOOP('',(#2095,#2096,#2097,#2098));
#501=EDGE_LOOP('',(#2099,#2100,#2101,#2102));
#502=EDGE_LOOP('',(#2103,#2104,#2105,#2106));
#503=EDGE_LOOP('',(#2107,#2108,#2109,#2110));
#504=EDGE_LOOP('',(#2111,#2112,#2113,#2114));
#505=EDGE_LOOP('',(#2115,#2116,#2117,#2118));
#506=EDGE_LOOP('',(#2119,#2120,#2121,#2122,#2123,#2124,#2125,#2126,#2127,
#2128,#2129,#2130,#2131,#2132,#2133,#2134));
#507=EDGE_LOOP('',(#2135,#2136,#2137,#2138,#2139,#2140,#2141,#2142,#2143,
#2144,#2145,#2146,#2147,#2148,#2149,#2150));
#508=EDGE_LOOP('',(#2151,#2152,#2153,#2154));
#509=EDGE_LOOP('',(#2155,#2156,#2157,#2158,#2159,#2160));
#510=EDGE_LOOP('',(#2161,#2162,#2163,#2164));
#511=EDGE_LOOP('',(#2165,#2166,#2167,#2168));
#512=EDGE_LOOP('',(#2169,#2170,#2171,#2172));
#513=EDGE_LOOP('',(#2173,#2174,#2175,#2176));
#514=EDGE_LOOP('',(#2177,#2178,#2179,#2180));
#515=EDGE_LOOP('',(#2181,#2182,#2183,#2184));
#516=EDGE_LOOP('',(#2185,#2186,#2187,#2188,#2189,#2190));
#517=EDGE_LOOP('',(#2191,#2192,#2193,#2194));
#518=LINE('',#3487,#656);
#519=LINE('',#3529,#657);
#520=LINE('',#3557,#658);
#521=LINE('',#3577,#659);
#522=LINE('',#3621,#660);
#523=LINE('',#3625,#661);
#524=LINE('',#3636,#662);
#525=LINE('',#3639,#663);
#526=LINE('',#3644,#664);
#527=LINE('',#3648,#665);
#528=LINE('',#3659,#666);
#529=LINE('',#3662,#667);
#530=LINE('',#3667,#668);
#531=LINE('',#3671,#669);
#532=LINE('',#3682,#670);
#533=LINE('',#3685,#671);
#534=LINE('',#3690,#672);
#535=LINE('',#3694,#673);
#536=LINE('',#3705,#674);
#537=LINE('',#3708,#675);
#538=LINE('',#3713,#676);
#539=LINE('',#3717,#677);
#540=LINE('',#3728,#678);
#541=LINE('',#3731,#679);
#542=LINE('',#3736,#680);
#543=LINE('',#3740,#681);
#544=LINE('',#3751,#682);
#545=LINE('',#3754,#683);
#546=LINE('',#3759,#684);
#547=LINE('',#3763,#685);
#548=LINE('',#3774,#686);
#549=LINE('',#3777,#687);
#550=LINE('',#3782,#688);
#551=LINE('',#3786,#689);
#552=LINE('',#3797,#690);
#553=LINE('',#3800,#691);
#554=LINE('',#3805,#692);
#555=LINE('',#3809,#693);
#556=LINE('',#3820,#694);
#557=LINE('',#3823,#695);
#558=LINE('',#3828,#696);
#559=LINE('',#3832,#697);
#560=LINE('',#3843,#698);
#561=LINE('',#3846,#699);
#562=LINE('',#3851,#700);
#563=LINE('',#3855,#701);
#564=LINE('',#3866,#702);
#565=LINE('',#3869,#703);
#566=LINE('',#3874,#704);
#567=LINE('',#3878,#705);
#568=LINE('',#3889,#706);
#569=LINE('',#3892,#707);
#570=LINE('',#3897,#708);
#571=LINE('',#3901,#709);
#572=LINE('',#3912,#710);
#573=LINE('',#3915,#711);
#574=LINE('',#3920,#712);
#575=LINE('',#3924,#713);
#576=LINE('',#3935,#714);
#577=LINE('',#3938,#715);
#578=LINE('',#3945,#716);
#579=LINE('',#3950,#717);
#580=LINE('',#3967,#718);
#581=LINE('',#3972,#719);
#582=LINE('',#3981,#720);
#583=LINE('',#3993,#721);
#584=LINE('',#3997,#722);
#585=LINE('',#3998,#723);
#586=LINE('',#4001,#724);
#587=LINE('',#4009,#725);
#588=LINE('',#4012,#726);
#589=LINE('',#4018,#727);
#590=LINE('',#4021,#728);
#591=LINE('',#4029,#729);
#592=LINE('',#4032,#730);
#593=LINE('',#4040,#731);
#594=LINE('',#4044,#732);
#595=LINE('',#4046,#733);
#596=LINE('',#4051,#734);
#597=LINE('',#4318,#735);
#598=LINE('',#4342,#736);
#599=LINE('',#4654,#737);
#600=LINE('',#4972,#738);
#601=LINE('',#5320,#739);
#602=LINE('',#5506,#740);
#603=LINE('',#5608,#741);
#604=LINE('',#5992,#742);
#605=LINE('',#6376,#743);
#606=LINE('',#6581,#744);
#607=LINE('',#6785,#745);
#608=LINE('',#8039,#746);
#609=LINE('',#8041,#747);
#610=LINE('',#8043,#748);
#611=LINE('',#8045,#749);
#612=LINE('',#8047,#750);
#613=LINE('',#8048,#751);
#614=LINE('',#8051,#752);
#615=LINE('',#8053,#753);
#616=LINE('',#8054,#754);
#617=LINE('',#8057,#755);
#618=LINE('',#8058,#756);
#619=LINE('',#8061,#757);
#620=LINE('',#8062,#758);
#621=LINE('',#8065,#759);
#622=LINE('',#8066,#760);
#623=LINE('',#8069,#761);
#624=LINE('',#8070,#762);
#625=LINE('',#8072,#763);
#626=LINE('',#8079,#764);
#627=LINE('',#8346,#765);
#628=LINE('',#8370,#766);
#629=LINE('',#8684,#767);
#630=LINE('',#9000,#768);
#631=LINE('',#9348,#769);
#632=LINE('',#9534,#770);
#633=LINE('',#9636,#771);
#634=LINE('',#10020,#772);
#635=LINE('',#10404,#773);
#636=LINE('',#10609,#774);
#637=LINE('',#10813,#775);
#638=LINE('',#12070,#776);
#639=LINE('',#12072,#777);
#640=LINE('',#12074,#778);
#641=LINE('',#12076,#779);
#642=LINE('',#12078,#780);
#643=LINE('',#12079,#781);
#644=LINE('',#12082,#782);
#645=LINE('',#12084,#783);
#646=LINE('',#12085,#784);
#647=LINE('',#12088,#785);
#648=LINE('',#12089,#786);
#649=LINE('',#12092,#787);
#650=LINE('',#12093,#788);
#651=LINE('',#12096,#789);
#652=LINE('',#12097,#790);
#653=LINE('',#12100,#791);
#654=LINE('',#12101,#792);
#655=LINE('',#12103,#793);
#656=VECTOR('',#2732,2.00054127207588);
#657=VECTOR('',#2737,2.50080065552765);
#658=VECTOR('',#2738,2.50080065552765);
#659=VECTOR('',#2743,2.00007126058529);
#660=VECTOR('',#2746,10.);
#661=VECTOR('',#2749,10.);
#662=VECTOR('',#2764,10.);
#663=VECTOR('',#2767,10.);
#664=VECTOR('',#2772,10.);
#665=VECTOR('',#2775,10.);
#666=VECTOR('',#2790,10.);
#667=VECTOR('',#2793,10.);
#668=VECTOR('',#2798,10.);
#669=VECTOR('',#2801,10.);
#670=VECTOR('',#2816,10.);
#671=VECTOR('',#2819,10.);
#672=VECTOR('',#2824,10.);
#673=VECTOR('',#2827,10.);
#674=VECTOR('',#2842,10.);
#675=VECTOR('',#2845,10.);
#676=VECTOR('',#2850,10.);
#677=VECTOR('',#2853,10.);
#678=VECTOR('',#2868,10.);
#679=VECTOR('',#2871,10.);
#680=VECTOR('',#2876,10.);
#681=VECTOR('',#2879,10.);
#682=VECTOR('',#2894,10.);
#683=VECTOR('',#2897,10.);
#684=VECTOR('',#2902,10.);
#685=VECTOR('',#2905,10.);
#686=VECTOR('',#2920,10.);
#687=VECTOR('',#2923,10.);
#688=VECTOR('',#2928,10.);
#689=VECTOR('',#2931,10.);
#690=VECTOR('',#2946,10.);
#691=VECTOR('',#2949,10.);
#692=VECTOR('',#2954,10.);
#693=VECTOR('',#2957,10.);
#694=VECTOR('',#2972,10.);
#695=VECTOR('',#2975,10.);
#696=VECTOR('',#2980,10.);
#697=VECTOR('',#2983,10.);
#698=VECTOR('',#2998,10.);
#699=VECTOR('',#3001,10.);
#700=VECTOR('',#3006,10.);
#701=VECTOR('',#3009,10.);
#702=VECTOR('',#3024,10.);
#703=VECTOR('',#3027,10.);
#704=VECTOR('',#3032,10.);
#705=VECTOR('',#3035,10.);
#706=VECTOR('',#3050,10.);
#707=VECTOR('',#3053,10.);
#708=VECTOR('',#3058,10.);
#709=VECTOR('',#3061,10.);
#710=VECTOR('',#3076,10.);
#711=VECTOR('',#3079,10.);
#712=VECTOR('',#3084,10.);
#713=VECTOR('',#3087,10.);
#714=VECTOR('',#3102,10.);
#715=VECTOR('',#3105,10.);
#716=VECTOR('',#3112,4.75930776765241);
#717=VECTOR('',#3117,10.);
#718=VECTOR('',#3148,10.);
#719=VECTOR('',#3153,10.);
#720=VECTOR('',#3166,10.);
#721=VECTOR('',#3183,6.82923606324244);
#722=VECTOR('',#3188,6.94701057265674);
#723=VECTOR('',#3189,6.94701057265674);
#724=VECTOR('',#3192,6.83201065632366);
#725=VECTOR('',#3203,4.80296382139185);
#726=VECTOR('',#3206,4.64521779108966);
#727=VECTOR('',#3215,2.61128051468949);
#728=VECTOR('',#3218,2.61559010295572);
#729=VECTOR('',#3229,4.64520588040018);
#730=VECTOR('',#3232,4.80503122320831);
#731=VECTOR('',#3243,6.83593993841137);
#732=VECTOR('',#3248,6.94665463816359);
#733=VECTOR('',#3251,6.82905809599587);
#734=VECTOR('',#3256,1.5555);
#735=VECTOR('',#3261,1.5555);
#736=VECTOR('',#3264,1.5555);
#737=VECTOR('',#3267,1.5555);
#738=VECTOR('',#3270,1.5555);
#739=VECTOR('',#3273,1.5555);
#740=VECTOR('',#3276,1.954);
#741=VECTOR('',#3281,1.954);
#742=VECTOR('',#3284,1.954);
#743=VECTOR('',#3287,1.954);
#744=VECTOR('',#3290,1.954);
#745=VECTOR('',#3293,1.954);
#746=VECTOR('',#3304,10.);
#747=VECTOR('',#3305,10.);
#748=VECTOR('',#3306,10.);
#749=VECTOR('',#3307,9.99999999999999);
#750=VECTOR('',#3308,10.);
#751=VECTOR('',#3309,10.);
#752=VECTOR('',#3312,10.);
#753=VECTOR('',#3313,10.);
#754=VECTOR('',#3314,10.);
#755=VECTOR('',#3317,10.);
#756=VECTOR('',#3318,10.);
#757=VECTOR('',#3321,10.);
#758=VECTOR('',#3322,10.);
#759=VECTOR('',#3325,10.);
#760=VECTOR('',#3326,9.99999999999999);
#761=VECTOR('',#3329,10.);
#762=VECTOR('',#3330,10.);
#763=VECTOR('',#3333,10.);
#764=VECTOR('',#3342,1.5555);
#765=VECTOR('',#3347,1.5555);
#766=VECTOR('',#3350,1.5555);
#767=VECTOR('',#3353,1.5555);
#768=VECTOR('',#3356,1.5555);
#769=VECTOR('',#3359,1.5555);
#770=VECTOR('',#3362,1.954);
#771=VECTOR('',#3367,1.954);
#772=VECTOR('',#3370,1.954);
#773=VECTOR('',#3373,1.954);
#774=VECTOR('',#3376,1.954);
#775=VECTOR('',#3379,1.954);
#776=VECTOR('',#3390,10.);
#777=VECTOR('',#3391,10.);
#778=VECTOR('',#3392,10.);
#779=VECTOR('',#3393,9.99999999999999);
#780=VECTOR('',#3394,10.);
#781=VECTOR('',#3395,10.);
#782=VECTOR('',#3398,10.);
#783=VECTOR('',#3399,10.);
#784=VECTOR('',#3400,10.);
#785=VECTOR('',#3403,10.);
#786=VECTOR('',#3404,10.);
#787=VECTOR('',#3407,10.);
#788=VECTOR('',#3408,10.);
#789=VECTOR('',#3411,10.);
#790=VECTOR('',#3412,9.99999999999999);
#791=VECTOR('',#3415,10.);
#792=VECTOR('',#3416,10.);
#793=VECTOR('',#3419,10.);
#794=B_SPLINE_CURVE_WITH_KNOTS('',3,(#3435,#3436,#3437,#3438,#3439,#3440,
#3441,#3442,#3443,#3444,#3445,#3446,#3447,#3448,#3449,#3450,#3451,#3452),
 .UNSPECIFIED.,.F.,.F.,(4,2,2,2,2,2,2,2,4),(-1.19269999759714,-1.12829413515979,
-1.04879502724507,-0.969295919330357,-0.889796811415643,-0.81029770350093,
-0.728247491527251,-0.687222385540411,-0.646197279553572),.UNSPECIFIED.);
#795=B_SPLINE_CURVE_WITH_KNOTS('',3,(#3454,#3455,#3456,#3457,#3458,#3459,
#3460,#3461,#3462,#3463,#3464,#3465,#3466,#3467),.UNSPECIFIED.,.F.,.F.,
(4,2,2,2,2,2,4),(-0.499257003558056,-0.483639998022121,-0.442252990706973,
-0.400865983391825,-0.359481492928847,-0.318097002465869,-0.302466663278823),
 .UNSPECIFIED.);
#796=B_SPLINE_CURVE_WITH_KNOTS('',3,(#3468,#3469,#3470,#3471,#3472,#3473,
#3474,#3475,#3476,#3477,#3478,#3479,#3480,#3481,#3482,#3483,#3484,#3485),
 .UNSPECIFIED.,.F.,.F.,(4,2,2,2,2,2,2,2,4),(-0.646197279553572,-0.605172173566732,
-0.564147067579893,-0.482096855606214,-0.4025977476915,-0.323098639776786,
-0.243599531862072,-0.164100423947358,-0.0997053765976701),
 .UNSPECIFIED.);
#797=B_SPLINE_CURVE_WITH_KNOTS('',3,(#3489,#3490,#3491,#3492,#3493,#3494,
#3495,#3496,#3497,#3498,#3499,#3500,#3501,#3502,#3503,#3504,#3505,#3506),
 .UNSPECIFIED.,.F.,.F.,(4,2,2,2,2,2,2,2,4),(0.,0.0758326534165654,0.151665306833131,
0.227478914786725,0.303292522740319,0.379106130693913,0.454919738647507,
0.530752392064072,0.606585045480638),.UNSPECIFIED.);
#798=B_SPLINE_CURVE_WITH_KNOTS('',3,(#3507,#3508,#3509,#3510,#3511,#3512,
#3513,#3514,#3515,#3516,#3517,#3518,#3519,#3520,#3521,#3522,#3523,#3524),
 .UNSPECIFIED.,.F.,.F.,(4,2,2,2,2,2,2,2,4),(0.606585045480638,0.682417698897203,
0.758250352313769,0.834063960267363,0.909877568220957,0.985691176174551,
1.06150478412814,1.13733743754471,1.21317009096128),.UNSPECIFIED.);
#799=B_SPLINE_CURVE_WITH_KNOTS('',3,(#3531,#3532,#3533,#3534,#3535,#3536,
#3537,#3538,#3539,#3540,#3541,#3542),.UNSPECIFIED.,.F.,.F.,(4,2,2,2,2,4),
(0.969015815726938,1.04849387615309,1.12797193657924,1.20999651210758,1.25100879987175,
1.29202108763592),.UNSPECIFIED.);
#800=B_SPLINE_CURVE_WITH_KNOTS('',3,(#3544,#3545,#3546,#3547,#3548,#3549,
#3550,#3551,#3552,#3553,#3554,#3555),.UNSPECIFIED.,.F.,.F.,(4,2,2,2,2,4),
(1.29202108763592,1.33303337540009,1.37404566316426,1.45607023869259,1.53554829911875,
1.6150263595449),.UNSPECIFIED.);
#801=B_SPLINE_CURVE_WITH_KNOTS('',3,(#3559,#3560,#3561,#3562,#3563,#3564,
#3565,#3566),.UNSPECIFIED.,.F.,.F.,(4,2,2,4),(1.6150263595449,1.69450441997105,
1.7739824803972,1.83833088236406),.UNSPECIFIED.);
#802=B_SPLINE_CURVE_WITH_KNOTS('',3,(#3567,#3568,#3569,#3570,#3571,#3572,
#3573,#3574),.UNSPECIFIED.,.F.,.F.,(4,2,2,4),(0.745700478002982,0.810059694874633,
0.889537755300786,0.969015815726938),.UNSPECIFIED.);
#803=B_SPLINE_CURVE_WITH_KNOTS('',3,(#3579,#3580,#3581,#3582,#3583,#3584,
#3585,#3586,#3587,#3588),.UNSPECIFIED.,.F.,.F.,(4,2,2,2,4),(0.909661063924676,
0.985456641432266,1.06125221893986,1.13706681875305,1.21288141856623),
 .UNSPECIFIED.);
#804=B_SPLINE_CURVE_WITH_KNOTS('',3,(#3590,#3591,#3592,#3593,#3594,#3595,
#3596,#3597,#3598,#3599,#3600,#3601,#3602,#3603,#3604,#3605,#3606,#3607),
 .UNSPECIFIED.,.F.,.F.,(4,2,2,2,2,2,2,2,4),(0.303220354641559,0.379015932149148,
0.454811509656738,0.530626109469928,0.606440709283118,0.682255309096307,
0.758069908909497,0.833865486417087,0.909661063924676),.UNSPECIFIED.);
#805=B_SPLINE_CURVE_WITH_KNOTS('',3,(#3608,#3609,#3610,#3611,#3612,#3613,
#3614,#3615,#3616,#3617),.UNSPECIFIED.,.F.,.F.,(4,2,2,2,4),(1.21288141856623,
1.28869601837942,1.36451061819261,1.4403061957002,1.51610177320779),
 .UNSPECIFIED.);
#806=B_SPLINE_CURVE_WITH_KNOTS('',3,(#4053,#4054,#4055,#4056,#4057,#4058,
#4059,#4060,#4061,#4062,#4063,#4064,#4065,#4066,#4067,#4068,#4069,#4070,
#4071,#4072,#4073,#4074,#4075,#4076,#4077,#4078,#4079,#4080,#4081,#4082,
#4083,#4084,#4085,#4086,#4087,#4088,#4089,#4090,#4091,#4092,#4093,#4094,
#4095,#4096,#4097,#4098,#4099,#4100,#4101,#4102,#4103,#4104,#4105,#4106,
#4107,#4108,#4109,#4110,#4111,#4112,#4113,#4114,#4115,#4116,#4117,#4118,
#4119,#4120,#4121,#4122,#4123,#4124,#4125,#4126,#4127,#4128,#4129,#4130,
#4131,#4132,#4133,#4134,#4135,#4136,#4137,#4138,#4139,#4140,#4141,#4142,
#4143,#4144,#4145,#4146,#4147,#4148,#4149,#4150,#4151,#4152,#4153,#4154,
#4155,#4156,#4157,#4158,#4159,#4160,#4161,#4162,#4163,#4164,#4165,#4166,
#4167,#4168,#4169,#4170,#4171,#4172,#4173,#4174,#4175,#4176,#4177,#4178,
#4179,#4180,#4181,#4182,#4183,#4184,#4185,#4186,#4187,#4188,#4189,#4190,
#4191,#4192,#4193,#4194,#4195,#4196,#4197,#4198,#4199,#4200),
 .UNSPECIFIED.,.F.,.F.,(4,3,3,3,3,3,3,3,3,3,3,3,3,3,3,3,3,3,3,3,3,3,3,3,
3,3,3,3,3,3,3,3,3,3,3,3,3,3,3,3,3,3,3,3,3,3,3,3,3,4),(10.3761213044057,
10.4916473343449,10.6020836926387,10.7124212898676,10.8227045964878,10.9329779958561,
11.0433574182079,11.153799603579,11.2644299007573,11.300329543919,11.412228455198,
11.5239351693938,11.6355347254554,11.7470696766159,11.8585824834667,11.9701986021098,
12.0818627300226,12.1937439049619,12.2969104176454,12.4084748637133,12.5198380200048,
12.6310887295725,12.7422701582708,12.8534253726942,12.9646803676604,13.0759808484134,
13.1874988487555,13.2934912913718,13.4052296275761,13.5167698094669,13.6281993328827,
13.7395610570682,13.8508977444198,13.9623346136355,14.07381749289,14.185516391903,
14.2900721650982,14.4018025327098,14.5133353791798,14.6247579576194,14.7361131396909,
14.8474437006735,14.9588751530413,15.0703529943082,15.182047571227,15.2866530388247,
15.4088138904719,15.5306080160377,15.6518307149662,15.7079632679489),
 .UNSPECIFIED.);
#807=B_SPLINE_CURVE_WITH_KNOTS('',3,(#4203,#4204,#4205,#4206,#4207,#4208,
#4209,#4210,#4211,#4212,#4213,#4214,#4215,#4216,#4217,#4218,#4219,#4220,
#4221,#4222,#4223,#4224,#4225,#4226,#4227,#4228,#4229,#4230,#4231,#4232,
#4233,#4234,#4235,#4236,#4237,#4238,#4239,#4240,#4241,#4242,#4243,#4244,
#4245,#4246,#4247,#4248,#4249,#4250,#4251,#4252,#4253,#4254,#4255,#4256,
#4257,#4258,#4259,#4260,#4261,#4262,#4263,#4264,#4265,#4266,#4267,#4268,
#4269,#4270,#4271,#4272,#4273,#4274,#4275,#4276,#4277,#4278,#4279,#4280,
#4281,#4282,#4283,#4284,#4285,#4286,#4287,#4288,#4289,#4290,#4291,#4292,
#4293,#4294,#4295,#4296,#4297,#4298,#4299,#4300,#4301,#4302,#4303,#4304,
#4305,#4306,#4307,#4308,#4309,#4310,#4311,#4312,#4313,#4314),
 .UNSPECIFIED.,.F.,.F.,(4,3,3,3,3,3,3,3,3,3,3,3,3,3,3,3,3,3,3,3,3,3,3,3,
3,3,3,3,3,3,3,3,3,3,3,3,3,4),(11.6154215191107,11.7297194433804,11.8439615074736,
11.9581751212632,12.0723949424661,12.1866556269815,12.3010886611519,12.4156103002373,
12.5303749287406,12.6120023928371,12.722600396268,12.8333482550549,12.9435980012706,
13.0537674854308,13.1639012473881,13.275071752182,13.3853379846654,13.4969606256144,
13.6085832665635,13.7204465169992,13.8321110831577,13.9436645730414,14.0551496181406,
14.16660875264,14.2781656624489,14.3897674585362,14.5015817699047,14.6051641402899,
14.7170632550792,14.8287701821625,14.9403699566644,15.051905131442,15.1634181667176,
15.2750345195736,15.386698885236,15.4985803008963,15.6017450140163,15.7079632679489),
 .UNSPECIFIED.);
#808=B_SPLINE_CURVE_WITH_KNOTS('',3,(#4319,#4320,#4321,#4322,#4323,#4324,
#4325,#4326,#4327,#4328),.UNSPECIFIED.,.F.,.F.,(4,1,1,1,1,1,1,4),(15.7079632679489,
16.2832339125511,17.2798147862775,18.2763956600039,19.2729765337303,20.2695574074567,
21.2661382811831,21.9911485751285),.UNSPECIFIED.);
#809=B_SPLINE_CURVE_WITH_KNOTS('',3,(#4329,#4330,#4331,#4332,#4333,#4334,
#4335,#4336,#4337,#4338),.UNSPECIFIED.,.F.,.F.,(4,1,1,1,1,1,1,4),(15.7079720007471,
16.5983258877427,17.5949067614691,18.5914876351955,19.5880685089219,20.5846493826483,
21.5812302563748,21.9911424371547),.UNSPECIFIED.);
#810=B_SPLINE_CURVE_WITH_KNOTS('',3,(#4343,#4344,#4345,#4346,#4347,#4348,
#4349,#4350,#4351,#4352,#4353,#4354,#4355,#4356,#4357,#4358,#4359,#4360,
#4361,#4362,#4363,#4364,#4365,#4366,#4367,#4368,#4369,#4370,#4371,#4372,
#4373,#4374,#4375,#4376,#4377,#4378,#4379,#4380,#4381,#4382,#4383,#4384,
#4385,#4386,#4387,#4388,#4389,#4390,#4391,#4392,#4393,#4394,#4395,#4396,
#4397,#4398,#4399,#4400,#4401,#4402,#4403,#4404,#4405,#4406,#4407,#4408,
#4409,#4410,#4411,#4412,#4413,#4414,#4415,#4416,#4417,#4418,#4419,#4420,
#4421,#4422,#4423,#4424,#4425,#4426,#4427,#4428,#4429,#4430,#4431,#4432,
#4433,#4434,#4435,#4436,#4437,#4438,#4439,#4440,#4441,#4442,#4443,#4444,
#4445,#4446,#4447,#4448,#4449,#4450,#4451,#4452,#4453,#4454,#4455,#4456,
#4457,#4458,#4459,#4460,#4461,#4462,#4463,#4464,#4465,#4466,#4467,#4468,
#4469,#4470,#4471,#4472,#4473,#4474,#4475,#4476,#4477,#4478,#4479,#4480,
#4481,#4482,#4483,#4484,#4485,#4486,#4487,#4488,#4489,#4490,#4491,#4492,
#4493,#4494,#4495,#4496,#4497,#4498,#4499,#4500,#4501,#4502,#4503,#4504,
#4505,#4506,#4507,#4508,#4509,#4510,#4511,#4512,#4513,#4514),
 .UNSPECIFIED.,.F.,.F.,(4,3,3,3,3,3,3,3,3,3,3,3,3,3,3,3,3,3,3,3,3,3,3,3,
3,3,3,3,3,3,3,3,3,3,3,3,3,3,3,3,3,3,3,3,3,3,3,3,3,3,3,3,3,3,3,3,3,4),(21.9911485751285,
22.1309179503363,22.2627191549095,22.374427659155,22.4859378873353,22.5973374041086,
22.708669121392,22.8199758541663,22.9313830961259,23.0428364782557,23.1545064918532,
23.2593000286359,23.3710083890299,23.4825184720439,23.5939178429524,23.7052494139272,
23.8165560002028,23.9279630965552,24.0394163333242,24.1510862038985,24.2558809023623,
24.3675891950941,24.479099207913,24.5904985071345,24.7018300050549,24.8131365170311,
24.9245435377139,25.0359966979394,25.1476664914795,25.2524617760888,25.3641701458249,
25.4756802374145,25.5870796164264,25.698411195018,25.8097177884088,25.9211248910232,
26.0325781335982,26.1442480091205,26.2490426498152,26.3607509985506,26.4722610688441,
26.5836604263951,26.6949919833986,26.8062985551115,26.9177056360823,27.0291588569968,
27.1408287111152,27.2456235235416,27.3573318547298,27.4688419071979,27.5802412467662,
27.6915727856601,27.8028793391664,27.9142864019218,28.0257396045861,28.1374094406315,
28.242204397268,28.2743338823081),.UNSPECIFIED.);
#811=B_SPLINE_CURVE_WITH_KNOTS('',3,(#4515,#4516,#4517,#4518,#4519,#4520,
#4521,#4522,#4523,#4524,#4525,#4526,#4527,#4528,#4529,#4530,#4531,#4532,
#4533,#4534,#4535,#4536,#4537,#4538,#4539,#4540,#4541,#4542,#4543,#4544,
#4545,#4546,#4547,#4548,#4549,#4550,#4551,#4552,#4553,#4554,#4555,#4556,
#4557,#4558,#4559,#4560,#4561,#4562,#4563,#4564,#4565,#4566,#4567,#4568,
#4569,#4570,#4571,#4572,#4573,#4574,#4575,#4576,#4577,#4578,#4579,#4580,
#4581,#4582,#4583,#4584,#4585,#4586,#4587,#4588,#4589,#4590,#4591,#4592,
#4593,#4594,#4595,#4596,#4597,#4598,#4599,#4600,#4601,#4602,#4603,#4604,
#4605,#4606,#4607,#4608,#4609,#4610,#4611,#4612,#4613,#4614,#4615,#4616,
#4617,#4618,#4619,#4620,#4621,#4622,#4623,#4624,#4625,#4626,#4627,#4628,
#4629,#4630,#4631,#4632,#4633,#4634,#4635,#4636,#4637,#4638,#4639,#4640,
#4641,#4642,#4643,#4644,#4645,#4646,#4647,#4648,#4649,#4650),
 .UNSPECIFIED.,.F.,.F.,(4,2,2,2,2,2,2,2,2,2,2,2,2,2,2,2,2,2,2,2,2,2,2,2,
2,2,2,2,2,2,2,2,2,2,2,2,2,2,2,2,2,2,2,2,2,2,2,2,2,2,2,2,2,2,2,2,2,2,2,2,
2,2,2,2,2,2,2,4),(-1.96082459543352,-1.95572351555056,-1.95066052951545,
-1.94362170361263,-1.93425075381217,-1.89502168228356,-1.87686387526354,
-1.87099759837285,-1.86650686710055,-1.85991368343642,-1.83588912387465,
-1.80491110925764,-1.79532103382858,-1.78754943506346,-1.77785045005196,
-1.7395832934319,-1.72145183028369,-1.71558876144544,-1.71109950362509,
-1.70450637904612,-1.67320765345622,-1.65092649870745,-1.64080239574451,
-1.63301540424833,-1.62377482636635,-1.58389582607512,-1.56598209910372,
-1.56013204953622,-1.55564145708863,-1.54903042008476,-1.52394393778717,
-1.50382039511072,-1.48957010087417,-1.481248627308,-1.47318169192042,-1.46067683095659,
-1.42781445661822,-1.41047349388771,-1.40466023251355,-1.40016532168693,
-1.39350050808931,-1.37077895797284,-1.34927674386887,-1.3385618526334,
-1.32899645945264,-1.32122258433739,-1.31149266274323,-1.27340973791122,
-1.25516680284208,-1.24929583368251,-1.24480601384231,-1.2382202508283,
-1.20684840126156,-1.18455492795627,-1.17444672041409,-1.16665843787414,
-1.15740148906793,-1.11777668409297,-1.09966402284823,-1.09380036224297,
-1.08930943635981,-1.08379516053843,-1.05304373469511,-1.02891096525692,
-1.01886083081681,-1.01107500165632,-1.00177403653395,-0.980700216948197),
 .UNSPECIFIED.);
#812=B_SPLINE_CURVE_WITH_KNOTS('',3,(#4655,#4656,#4657,#4658,#4659,#4660,
#4661,#4662,#4663,#4664,#4665,#4666,#4667,#4668,#4669,#4670,#4671,#4672,
#4673,#4674,#4675,#4676,#4677,#4678,#4679,#4680,#4681,#4682,#4683,#4684,
#4685,#4686,#4687,#4688,#4689,#4690,#4691,#4692,#4693,#4694,#4695,#4696,
#4697,#4698,#4699,#4700,#4701,#4702,#4703,#4704,#4705,#4706,#4707,#4708,
#4709,#4710,#4711,#4712,#4713,#4714,#4715,#4716,#4717,#4718,#4719,#4720,
#4721,#4722,#4723,#4724,#4725,#4726,#4727,#4728,#4729,#4730,#4731,#4732,
#4733,#4734,#4735,#4736,#4737,#4738,#4739,#4740,#4741,#4742,#4743,#4744,
#4745,#4746,#4747,#4748,#4749,#4750,#4751,#4752,#4753,#4754,#4755,#4756,
#4757,#4758,#4759,#4760,#4761,#4762,#4763,#4764,#4765,#4766,#4767,#4768,
#4769,#4770,#4771,#4772,#4773,#4774,#4775,#4776,#4777,#4778,#4779,#4780,
#4781,#4782,#4783,#4784,#4785,#4786,#4787,#4788,#4789,#4790,#4791,#4792,
#4793,#4794,#4795,#4796,#4797,#4798,#4799,#4800,#4801,#4802,#4803,#4804,
#4805,#4806,#4807,#4808,#4809,#4810,#4811,#4812,#4813,#4814,#4815,#4816,
#4817,#4818,#4819,#4820,#4821,#4822,#4823,#4824,#4825,#4826),
 .UNSPECIFIED.,.F.,.F.,(4,3,3,3,3,3,3,3,3,3,3,3,3,3,3,3,3,3,3,3,3,3,3,3,
3,3,3,3,3,3,3,3,3,3,3,3,3,3,3,3,3,3,3,3,3,3,3,3,3,3,3,3,3,3,3,3,3,4),(28.2743338828609,
28.3854499463251,28.4963720118463,28.6071867805496,28.717938100074,28.8286697232355,
28.9395040413308,29.0503910293876,29.1614837232969,29.2387852709944,29.3504936415299,
29.4620037336246,29.5734031129626,29.6847346917021,29.7960412850626,29.9074483873678,
30.0189016294807,30.1305715042882,30.2353661447208,30.3470744333654,30.4585844436019,
30.5699837411555,30.6813152383202,30.7926217504514,30.9040287727148,31.0154819353027,
31.1271517324973,31.2319470184472,31.3436553843173,31.4551654707913,31.5665648439343,
31.6778964159217,31.7892030019896,31.9006100962241,32.012063329828,32.123733195506,
32.2285278921736,32.340236400346,32.4517466310075,32.5631461493832,32.6744778673927,
32.785784600018,32.8971918404589,33.008645220319,33.1203152304053,33.2251087659,
33.3368166944273,33.448326345267,33.5597252840979,33.6710564238064,33.782362580341,
33.8937692527465,34.0052220680337,34.1168915267859,34.2216896396264,34.3523579101837,
34.481718471603,34.5575191891205),.UNSPECIFIED.);
#813=B_SPLINE_CURVE_WITH_KNOTS('',3,(#4827,#4828,#4829,#4830,#4831,#4832,
#4833,#4834,#4835,#4836,#4837,#4838,#4839,#4840,#4841,#4842,#4843,#4844,
#4845,#4846,#4847,#4848,#4849,#4850,#4851,#4852,#4853,#4854,#4855,#4856,
#4857,#4858,#4859,#4860,#4861,#4862,#4863,#4864,#4865,#4866,#4867,#4868,
#4869,#4870,#4871,#4872,#4873,#4874,#4875,#4876,#4877,#4878,#4879,#4880,
#4881,#4882,#4883,#4884,#4885,#4886,#4887,#4888,#4889,#4890,#4891,#4892,
#4893,#4894,#4895,#4896,#4897,#4898,#4899,#4900,#4901,#4902,#4903,#4904,
#4905,#4906,#4907,#4908,#4909,#4910,#4911,#4912,#4913,#4914,#4915,#4916,
#4917,#4918,#4919,#4920,#4921,#4922,#4923,#4924,#4925,#4926,#4927,#4928,
#4929,#4930,#4931,#4932,#4933,#4934,#4935,#4936,#4937,#4938,#4939,#4940,
#4941,#4942,#4943,#4944,#4945,#4946,#4947,#4948,#4949,#4950,#4951,#4952,
#4953,#4954,#4955,#4956,#4957,#4958,#4959,#4960,#4961,#4962,#4963,#4964,
#4965,#4966,#4967,#4968),.UNSPECIFIED.,.F.,.F.,(4,2,2,2,2,2,2,2,2,2,2,2,
2,2,2,2,2,2,2,2,2,2,2,2,2,2,2,2,2,2,2,2,2,2,2,2,2,2,2,2,2,2,2,2,2,2,2,2,
2,2,2,2,2,2,2,2,2,2,2,2,2,2,2,2,2,2,2,2,2,2,4),(-0.980700216948197,-0.980559999268628,
-0.955579621572852,-0.943370892251875,-0.937835489269082,-0.933291897005555,
-0.926150713138604,-0.916953615712503,-0.891349546080903,-0.871223254441055,
-0.861966129363549,-0.854176350201917,-0.844064404906459,-0.821753526458986,
-0.790354057030155,-0.783765544398651,-0.779274810972388,-0.77340375146535,
-0.755163698290188,-0.717100806565004,-0.707370007481461,-0.699594528982264,
-0.690026074686523,-0.661308930911707,-0.634689541588939,-0.628178275122494,
-0.623692439346925,-0.617763729956392,-0.598443836723945,-0.562381120374292,
-0.552467797355895,-0.544680065830786,-0.535405586845253,-0.512220539516689,
-0.478626029675242,-0.472375693210019,-0.467898681844763,-0.461744853680482,
-0.437725670751447,-0.407116607316036,-0.397117959937511,-0.389324669566922,
-0.380112242331538,-0.357849119206682,-0.324943098177345,-0.317823703984556,
-0.313282767370483,-0.307736107332356,-0.293540257053314,-0.262376920178938,
-0.246674845683532,-0.238147767728558,-0.230193327463652,-0.218508298981253,
-0.20401103902391,-0.179203341412983,-0.165928827760339,-0.160404579058862,
-0.155858235240732,-0.14869449556963,-0.139455516781709,-0.113568526872797,
-0.093603434538257,-0.0844122465129277,-0.0766165286016932,-0.0664092592360509,
-0.041010860894887,-0.0117519087702631,-0.00581551109514165,-0.00289996074689045,
-0.000457478146548932),.UNSPECIFIED.);
#814=B_SPLINE_CURVE_WITH_KNOTS('',3,(#4973,#4974,#4975,#4976,#4977,#4978,
#4979,#4980,#4981,#4982,#4983,#4984,#4985,#4986,#4987,#4988,#4989,#4990,
#4991,#4992,#4993,#4994,#4995,#4996,#4997,#4998,#4999,#5000,#5001,#5002,
#5003,#5004,#5005,#5006,#5007,#5008,#5009,#5010,#5011,#5012,#5013,#5014,
#5015,#5016,#5017,#5018,#5019,#5020,#5021,#5022,#5023,#5024,#5025,#5026,
#5027,#5028,#5029,#5030,#5031,#5032,#5033,#5034,#5035,#5036,#5037,#5038,
#5039,#5040,#5041,#5042,#5043,#5044,#5045,#5046,#5047,#5048,#5049,#5050,
#5051,#5052,#5053,#5054,#5055,#5056,#5057,#5058,#5059,#5060,#5061,#5062,
#5063,#5064,#5065,#5066,#5067,#5068,#5069,#5070,#5071,#5072,#5073,#5074,
#5075,#5076,#5077,#5078,#5079,#5080,#5081,#5082,#5083,#5084,#5085,#5086,
#5087,#5088,#5089,#5090,#5091,#5092,#5093,#5094,#5095,#5096,#5097,#5098,
#5099,#5100,#5101,#5102,#5103,#5104,#5105,#5106,#5107,#5108,#5109,#5110,
#5111,#5112,#5113,#5114,#5115,#5116,#5117,#5118,#5119,#5120,#5121,#5122,
#5123,#5124,#5125,#5126,#5127,#5128,#5129,#5130,#5131,#5132,#5133,#5134,
#5135,#5136,#5137,#5138,#5139,#5140,#5141,#5142,#5143,#5144),
 .UNSPECIFIED.,.F.,.F.,(4,3,3,3,3,3,3,3,3,3,3,3,3,3,3,3,3,3,3,3,3,3,3,3,
3,3,3,3,3,3,3,3,3,3,3,3,3,3,3,3,3,3,3,3,3,3,3,3,3,3,3,3,3,3,3,3,3,4),(34.5575191894877,
34.6688302723381,34.7801258851519,34.8915360000218,35.0030001705124,35.1146924423317,
35.2182705133528,35.329979844159,35.4414909051851,35.5528912580536,35.6642238132373,
35.7755313842774,35.8869394583063,35.9983936704943,36.1100644998149,36.2148513870793,
36.3265566868323,36.4380637110229,36.5494600262282,36.660788549687,36.7720921017016,
36.8834962086944,36.9949464756926,37.1066134484121,37.2114322608057,37.3231433221254,
37.4346560660442,37.5460580718723,37.6573922476747,37.7687014045501,37.8801109978222,
37.9915666953808,38.1032389338652,38.2080131345321,38.3197270786043,38.4312428141906,
38.5426478756073,38.6539851650299,38.7652974877472,38.8767103021911,38.9881692564663,
39.0998447680598,39.2045940082585,39.3162806032607,39.4277689172748,39.5391465312969,
39.6504563936481,39.7617413557063,39.8731271322649,39.9845591801971,40.0962083605028,
40.2011748819849,40.31341306353,40.4254718990605,40.5373841223233,40.6492090027682,
40.7610153241073,40.8407044966673),.UNSPECIFIED.);
#815=B_SPLINE_CURVE_WITH_KNOTS('',3,(#5145,#5146,#5147,#5148,#5149,#5150,
#5151,#5152,#5153,#5154,#5155,#5156,#5157,#5158,#5159,#5160,#5161,#5162,
#5163,#5164,#5165,#5166,#5167,#5168,#5169,#5170,#5171,#5172,#5173,#5174,
#5175,#5176,#5177,#5178,#5179,#5180,#5181,#5182,#5183,#5184,#5185,#5186,
#5187,#5188,#5189,#5190,#5191,#5192,#5193,#5194,#5195,#5196,#5197,#5198,
#5199,#5200,#5201,#5202,#5203,#5204,#5205,#5206,#5207,#5208,#5209,#5210,
#5211,#5212,#5213,#5214,#5215,#5216,#5217,#5218,#5219,#5220,#5221,#5222,
#5223,#5224,#5225,#5226,#5227,#5228,#5229,#5230,#5231,#5232,#5233,#5234,
#5235,#5236,#5237,#5238,#5239,#5240,#5241,#5242,#5243,#5244,#5245,#5246,
#5247,#5248,#5249,#5250,#5251,#5252,#5253,#5254,#5255,#5256,#5257,#5258,
#5259,#5260,#5261,#5262,#5263,#5264,#5265,#5266,#5267,#5268,#5269,#5270,
#5271,#5272,#5273,#5274,#5275,#5276,#5277,#5278,#5279,#5280,#5281,#5282,
#5283,#5284,#5285,#5286,#5287,#5288,#5289,#5290,#5291,#5292,#5293,#5294,
#5295,#5296,#5297,#5298,#5299,#5300,#5301,#5302,#5303,#5304,#5305,#5306,
#5307,#5308,#5309,#5310,#5311,#5312,#5313,#5314,#5315,#5316),
 .UNSPECIFIED.,.F.,.F.,(4,3,3,3,3,3,3,3,3,3,3,3,3,3,3,3,3,3,3,3,3,3,3,3,
3,3,3,3,3,3,3,3,3,3,3,3,3,3,3,3,3,3,3,3,3,3,3,3,3,3,3,3,3,3,3,3,3,4),(34.557519189864,
34.6688316922454,34.7799480549331,34.8909555466977,35.0018977265955,35.1128180578457,
35.2238400790168,35.3349122896089,35.4461940347628,35.5333624885445,35.6450709986201,
35.7565812311951,35.8679807514893,35.979312471419,36.0906192059629,36.2020264483048,
36.3134798300592,36.4251498420041,36.5299433622709,36.6416512870095,36.7531609340693,
36.8645598691282,36.9758910050783,37.0871971578744,37.1986038266027,37.3100566382398,
37.4217260934355,37.5265242359973,37.6382328481534,37.7497431759177,37.861142787168,
37.9724745937193,38.083781410444,38.1951887274328,38.3066421798416,38.4183122548368,
38.5231051097237,38.634814450544,38.7463255216521,38.8577258846372,38.9690584499546,
39.0803660311284,39.19177411521,39.3032283374232,39.4148991765908,39.5196859834501,
39.6313912609589,39.742898262931,39.8542945559478,39.9656230572846,40.0769265872801,
40.1883306725883,40.2997809180488,40.4114478697594,40.5162668571765,40.6484523927198,
40.7791766765676,40.8407044966673),.UNSPECIFIED.);
#816=B_SPLINE_CURVE_WITH_KNOTS('',3,(#5321,#5322,#5323,#5324,#5325,#5326,
#5327,#5328,#5329,#5330,#5331,#5332,#5333,#5334,#5335,#5336,#5337,#5338,
#5339,#5340,#5341,#5342,#5343,#5344,#5345,#5346,#5347,#5348,#5349,#5350,
#5351,#5352,#5353,#5354,#5355,#5356,#5357,#5358,#5359,#5360,#5361,#5362,
#5363,#5364,#5365,#5366,#5367,#5368,#5369,#5370,#5371,#5372,#5373,#5374,
#5375,#5376,#5377,#5378,#5379,#5380,#5381,#5382,#5383,#5384,#5385,#5386,
#5387,#5388,#5389,#5390,#5391,#5392,#5393,#5394,#5395,#5396,#5397,#5398,
#5399,#5400,#5401,#5402,#5403,#5404,#5405,#5406,#5407,#5408,#5409,#5410,
#5411,#5412,#5413,#5414,#5415,#5416,#5417,#5418,#5419,#5420,#5421,#5422,
#5423,#5424,#5425,#5426,#5427,#5428,#5429,#5430,#5431,#5432,#5433,#5434,
#5435,#5436,#5437,#5438,#5439,#5440,#5441,#5442,#5443,#5444,#5445,#5446,
#5447,#5448,#5449,#5450,#5451,#5452,#5453,#5454,#5455,#5456,#5457,#5458,
#5459,#5460,#5461,#5462,#5463,#5464,#5465,#5466,#5467,#5468,#5469,#5470,
#5471,#5472,#5473,#5474,#5475,#5476,#5477,#5478,#5479,#5480,#5481,#5482,
#5483,#5484,#5485,#5486,#5487,#5488,#5489,#5490,#5491,#5492),
 .UNSPECIFIED.,.F.,.F.,(4,3,3,3,3,3,3,3,3,3,3,3,3,3,3,3,3,3,3,3,3,3,3,3,
3,3,3,3,3,3,3,3,3,3,3,3,3,3,3,3,3,3,3,3,3,3,3,3,3,3,3,3,3,3,3,3,3,4),(40.840704497049,
40.9675412582681,41.0954926672067,41.1977557557113,41.3094929575612,41.4210324227689,
41.5324614834252,41.643822998072,41.755159728709,41.8665970369414,41.9780805721874,
42.0897804857432,42.1943366294377,42.3058933565765,42.4172516335833,42.5284991889106,
42.6396791835826,42.750834681469,42.8620926517494,42.9733975818198,43.0849224744629,
43.1909175031641,43.3028373726712,43.4145573215696,43.5261654134577,43.6377042144518,
43.7492161924285,43.8608241682442,43.972476138112,44.0843385386926,44.1874983768905,
44.2993486307196,44.4110045193044,44.5225519596468,44.6340335782541,44.7454919074657,
44.8570521214737,44.9686594749185,45.0804830762105,45.1840792506169,45.2946069224391,
45.4053635726771,45.5155858115154,45.6257438851438,45.7358823024636,45.8470767579335,
45.9573868777162,46.0690235010298,46.1806601243433,46.2985638342812,46.4122814276395,
46.5258600264502,46.6393375177505,46.7527516466315,46.8661750751564,46.9796037930556,
47.09312121241,47.1238898038469),.UNSPECIFIED.);
#817=B_SPLINE_CURVE_WITH_KNOTS('',3,(#5493,#5494,#5495,#5496,#5497,#5498,
#5499,#5500,#5501,#5502),.UNSPECIFIED.,.F.,.F.,(4,1,1,1,1,1,1,4),(40.8407044966673,
41.5128477309029,42.5094286046293,43.5060094783558,44.5025903520822,45.4991712258086,
46.495752099535,47.1238898038469),.UNSPECIFIED.);
#818=B_SPLINE_CURVE_WITH_KNOTS('',3,(#5508,#5509,#5510,#5511,#5512,#5513,
#5514,#5515,#5516,#5517,#5518,#5519,#5520,#5521,#5522,#5523,#5524,#5525,
#5526,#5527,#5528,#5529,#5530,#5531,#5532,#5533,#5534,#5535,#5536,#5537,
#5538,#5539,#5540,#5541,#5542,#5543,#5544,#5545,#5546,#5547,#5548,#5549,
#5550,#5551,#5552,#5553,#5554,#5555,#5556,#5557,#5558,#5559,#5560,#5561,
#5562,#5563,#5564,#5565,#5566,#5567,#5568),.UNSPECIFIED.,.F.,.F.,(4,3,3,
3,3,3,3,3,3,3,3,3,3,3,3,3,3,3,3,3,4),(-4.09254174883831,-3.98632349490564,
-3.88060657601914,-3.77504892759548,-3.66961679425284,-3.56425173722798,
-3.45891795737595,-3.35357970118941,-3.24813369183697,-3.14262668426919,
-3.03694351958987,-2.98974262117923,-2.88522737486619,-2.78088717581068,
-2.67664451339598,-2.5724618858615,-2.46830187348436,-2.36405791614848,
-2.25977409419917,-2.15530886452126,-2.0655090872996),.UNSPECIFIED.);
#819=B_SPLINE_CURVE_WITH_KNOTS('',3,(#5571,#5572,#5573,#5574,#5575,#5576,
#5577,#5578,#5579,#5580,#5581,#5582,#5583,#5584,#5585,#5586,#5587,#5588,
#5589,#5590,#5591,#5592,#5593,#5594,#5595,#5596,#5597,#5598,#5599,#5600,
#5601,#5602,#5603,#5604),.UNSPECIFIED.,.F.,.F.,(4,3,3,3,3,3,3,3,3,3,3,4),
(0.,0.107961337641777,0.219038779652356,0.32692137897961,0.434806064728328,
0.542722047025844,0.656186753700985,0.764334836393942,0.872582285248764,
0.981026153163086,0.996580873726409,1.11419103802958),.UNSPECIFIED.);
#820=B_SPLINE_CURVE_WITH_KNOTS('',3,(#5609,#5610,#5611,#5612,#5613,#5614,
#5615,#5616,#5617,#5618,#5619,#5620,#5621,#5622,#5623,#5624,#5625,#5626,
#5627,#5628,#5629,#5630,#5631,#5632,#5633,#5634,#5635,#5636,#5637,#5638,
#5639,#5640,#5641,#5642,#5643,#5644,#5645,#5646,#5647,#5648,#5649,#5650,
#5651,#5652,#5653,#5654,#5655,#5656,#5657,#5658,#5659,#5660,#5661,#5662,
#5663,#5664,#5665,#5666,#5667,#5668,#5669,#5670,#5671,#5672,#5673,#5674,
#5675,#5676,#5677,#5678,#5679,#5680,#5681,#5682,#5683,#5684,#5685,#5686,
#5687,#5688,#5689,#5690,#5691,#5692,#5693,#5694,#5695,#5696,#5697,#5698,
#5699,#5700,#5701,#5702,#5703,#5704,#5705,#5706,#5707,#5708,#5709,#5710,
#5711,#5712,#5713,#5714,#5715,#5716,#5717,#5718,#5719,#5720,#5721,#5722,
#5723,#5724,#5725,#5726,#5727,#5728,#5729,#5730,#5731,#5732,#5733,#5734,
#5735,#5736,#5737,#5738,#5739,#5740,#5741,#5742,#5743,#5744,#5745,#5746,
#5747,#5748,#5749,#5750,#5751,#5752,#5753,#5754,#5755,#5756,#5757,#5758,
#5759,#5760,#5761,#5762,#5763,#5764,#5765,#5766,#5767,#5768,#5769,#5770,
#5771,#5772,#5773,#5774,#5775,#5776,#5777,#5778,#5779,#5780,#5781,#5782,
#5783,#5784,#5785,#5786,#5787,#5788,#5789,#5790,#5791,#5792,#5793,#5794,
#5795,#5796,#5797,#5798),.UNSPECIFIED.,.F.,.F.,(4,3,3,3,3,3,3,3,3,3,3,3,
3,3,3,3,3,3,3,3,3,3,3,3,3,3,3,3,3,3,3,3,3,3,3,3,3,3,3,3,3,3,3,3,3,3,3,3,
3,3,3,3,3,3,3,3,3,3,3,3,3,3,3,4),(-10.3757270556279,-10.2603201973078,-10.1445336437559,
-10.0282150027604,-9.96580873726409,-9.86028927215325,-9.75492847331706,
-9.6496913482242,-9.54452003581519,-9.43937844760697,-9.33423053922643,
-9.22897081685296,-9.12364803666887,-9.01814404094803,-8.96922786353768,
-8.863705637873,-8.75834200872326,-8.65310196527414,-8.5479276817438,-8.44278307461428,
-8.33763210442475,-8.23236927738943,-8.12704336360682,-8.02153622334531,
-7.97264698981127,-7.86715075765799,-7.76181321062034,-7.65659925346559,
-7.55145104369271,-7.44633245870662,-7.34120741993231,-7.23597021141748,
-7.13066977480087,-7.02518762842017,-6.97606611608487,-6.87052576919234,
-6.76514418013919,-6.65988649813286,-6.55469478529851,-6.44953298257141,
-6.34436507518076,-6.23908581202832,-6.13374372441398,-6.02822097903253,
-5.97948524235845,-5.87394087033655,-5.7685547754276,-5.66329190907336,
-5.55809459516585,-5.45292678697878,-5.34775248164716,-5.24246628022611,
-5.13711693603417,-5.0315865271823,-4.98290436863205,-4.87887809662517,
-4.77503069661954,-4.67128271432362,-4.56759611534957,-4.46393295588717,
-4.36019408038188,-4.25641481532166,-4.15247510001585,-4.09254174928665),
 .UNSPECIFIED.);
#821=B_SPLINE_CURVE_WITH_KNOTS('',3,(#5799,#5800,#5801,#5802,#5803,#5804,
#5805,#5806,#5807,#5808,#5809,#5810,#5811,#5812,#5813,#5814,#5815,#5816,
#5817,#5818,#5819,#5820,#5821,#5822,#5823,#5824,#5825,#5826,#5827,#5828,
#5829,#5830,#5831,#5832,#5833,#5834,#5835,#5836,#5837,#5838,#5839,#5840,
#5841,#5842,#5843,#5844,#5845,#5846,#5847,#5848,#5849,#5850,#5851,#5852,
#5853,#5854,#5855,#5856,#5857,#5858,#5859,#5860,#5861,#5862,#5863,#5864,
#5865,#5866,#5867,#5868,#5869,#5870,#5871,#5872,#5873,#5874,#5875,#5876,
#5877,#5878,#5879,#5880,#5881,#5882,#5883,#5884,#5885,#5886,#5887,#5888,
#5889,#5890,#5891,#5892,#5893,#5894,#5895,#5896,#5897,#5898,#5899,#5900,
#5901,#5902,#5903,#5904,#5905,#5906,#5907,#5908,#5909,#5910,#5911,#5912,
#5913,#5914,#5915,#5916,#5917,#5918,#5919,#5920,#5921,#5922,#5923,#5924,
#5925,#5926,#5927,#5928,#5929,#5930,#5931,#5932,#5933,#5934,#5935,#5936,
#5937,#5938,#5939,#5940,#5941,#5942,#5943,#5944,#5945,#5946,#5947,#5948,
#5949,#5950,#5951,#5952,#5953,#5954,#5955,#5956,#5957,#5958,#5959,#5960,
#5961,#5962,#5963,#5964,#5965,#5966,#5967,#5968,#5969,#5970,#5971,#5972,
#5973,#5974,#5975,#5976,#5977,#5978,#5979,#5980,#5981,#5982,#5983,#5984,
#5985,#5986,#5987,#5988),.UNSPECIFIED.,.F.,.F.,(4,3,3,3,3,3,3,3,3,3,3,3,
3,3,3,3,3,3,3,3,3,3,3,3,3,3,3,3,3,3,3,3,3,3,3,3,3,3,3,3,3,3,3,3,3,3,3,3,
3,3,3,3,3,3,3,3,3,3,3,3,3,3,3,4),(1.1141910384302,1.2172423853623,1.32013451940761,
1.42293952840393,1.52569615018631,1.62844303717393,1.73128762649985,1.83418552892848,
1.93726302853859,1.99316174745282,2.09882380530123,2.20432723759872,2.30970630945708,
2.41501904637488,2.52030130546144,2.62558889901074,2.73098582593685,2.83644458423473,
2.94208122698995,2.98974262117923,3.09543951511609,3.20098166055251,3.30640502061644,
3.41176548868153,3.51709885740485,3.62244087819006,3.72789690172125,3.83341751347036,
3.93911962813814,3.98632349490564,4.09170446142591,4.19692477051415,4.30201914206343,
4.40704637515926,4.51204277383519,4.61704459671689,4.72215786837964,4.82733377202005,
4.93269176979819,4.98290436863205,5.08844958739663,5.19383628319028,5.29909938551086,
5.40429670879892,5.50946430050002,5.61463816395977,5.71992358734206,5.82527196030871,
5.93080111180717,5.97948524235846,6.08502293419111,6.19040246033158,6.29565896133585,
6.40085004111375,6.50601175791141,6.61118012626036,6.71646067026059,6.82180450898163,
6.92732970844788,6.97606611608486,7.09145618049362,7.20651961582521,7.32105406185248,
7.39737634485402),.UNSPECIFIED.);
#822=B_SPLINE_CURVE_WITH_KNOTS('',3,(#5993,#5994,#5995,#5996,#5997,#5998,
#5999,#6000,#6001,#6002,#6003,#6004,#6005,#6006,#6007,#6008,#6009,#6010,
#6011,#6012,#6013,#6014,#6015,#6016,#6017,#6018,#6019,#6020,#6021,#6022,
#6023,#6024,#6025,#6026,#6027,#6028,#6029,#6030,#6031,#6032,#6033,#6034,
#6035,#6036,#6037,#6038,#6039,#6040,#6041,#6042,#6043,#6044,#6045,#6046,
#6047,#6048,#6049,#6050,#6051,#6052,#6053,#6054,#6055,#6056,#6057,#6058,
#6059,#6060,#6061,#6062,#6063,#6064,#6065,#6066,#6067,#6068,#6069,#6070,
#6071,#6072,#6073,#6074,#6075,#6076,#6077,#6078,#6079,#6080,#6081,#6082,
#6083,#6084,#6085,#6086,#6087,#6088,#6089,#6090,#6091,#6092,#6093,#6094,
#6095,#6096,#6097,#6098,#6099,#6100,#6101,#6102,#6103,#6104,#6105,#6106,
#6107,#6108,#6109,#6110,#6111,#6112,#6113,#6114,#6115,#6116,#6117,#6118,
#6119,#6120,#6121,#6122,#6123,#6124,#6125,#6126,#6127,#6128,#6129,#6130,
#6131,#6132,#6133,#6134,#6135,#6136,#6137,#6138,#6139,#6140,#6141,#6142,
#6143,#6144,#6145,#6146,#6147,#6148,#6149,#6150,#6151,#6152,#6153,#6154,
#6155,#6156,#6157,#6158,#6159,#6160,#6161,#6162,#6163,#6164,#6165,#6166,
#6167,#6168,#6169,#6170,#6171,#6172,#6173,#6174,#6175,#6176,#6177,#6178,
#6179,#6180,#6181,#6182),.UNSPECIFIED.,.F.,.F.,(4,3,3,3,3,3,3,3,3,3,3,3,
3,3,3,3,3,3,3,3,3,3,3,3,3,3,3,3,3,3,3,3,3,3,3,3,3,3,3,3,3,3,3,3,3,3,3,3,
3,3,3,3,3,3,3,3,3,3,3,3,3,3,3,4),(-16.6589123631975,-16.5545511958811,-16.4502386019146,
-16.3459373792314,-16.2415362416229,-16.1370858710382,-16.0324418402438,
-15.9452939796226,-15.8397770700369,-15.7344188085271,-15.6291841820782,
-15.5240153429196,-15.4188761990733,-15.3137307026422,-15.2084733274024,
-15.1031528607634,-14.9976511031841,-14.9487131058961,-14.8431960601416,
-14.7378376610967,-14.6326028957817,-14.5274339170146,-14.4222946330345,
-14.3171489961609,-14.2118914809823,-14.1065708744895,-14.0010689786591,
-13.9521322321697,-13.8466157393099,-13.7412578942319,-13.6360236817895,
-13.5308552548953,-13.4257165209662,-13.3205714314978,-13.2153144560295,
-13.1099943856373,-13.0044930147745,-12.9555513584433,-12.8500342162662,
-12.7446757247134,-12.6394408730378,-12.5342718117637,-12.4291324492194,
-12.3239867378176,-12.2187291546321,-12.1134084837551,-12.0079065297222,
-11.9589704847169,-11.853452654262,-11.7480934645292,-11.642857903596,-11.5376881266249,
-11.432548043081,-11.3274016065084,-11.2221432969163,-11.1168218978765,
-11.0113192206858,-10.9623896109905,-10.8549891203279,-10.7477671220514,
-10.6407197315394,-10.533774763467,-10.4269036873042,-10.3757270560179),
 .UNSPECIFIED.);
#823=B_SPLINE_CURVE_WITH_KNOTS('',3,(#6183,#6184,#6185,#6186,#6187,#6188,
#6189,#6190,#6191,#6192,#6193,#6194,#6195,#6196,#6197,#6198,#6199,#6200,
#6201,#6202,#6203,#6204,#6205,#6206,#6207,#6208,#6209,#6210,#6211,#6212,
#6213,#6214,#6215,#6216,#6217,#6218,#6219,#6220,#6221,#6222,#6223,#6224,
#6225,#6226,#6227,#6228,#6229,#6230,#6231,#6232,#6233,#6234,#6235,#6236,
#6237,#6238,#6239,#6240,#6241,#6242,#6243,#6244,#6245,#6246,#6247,#6248,
#6249,#6250,#6251,#6252,#6253,#6254,#6255,#6256,#6257,#6258,#6259,#6260,
#6261,#6262,#6263,#6264,#6265,#6266,#6267,#6268,#6269,#6270,#6271,#6272,
#6273,#6274,#6275,#6276,#6277,#6278,#6279,#6280,#6281,#6282,#6283,#6284,
#6285,#6286,#6287,#6288,#6289,#6290,#6291,#6292,#6293,#6294,#6295,#6296,
#6297,#6298,#6299,#6300,#6301,#6302,#6303,#6304,#6305,#6306,#6307,#6308,
#6309,#6310,#6311,#6312,#6313,#6314,#6315,#6316,#6317,#6318,#6319,#6320,
#6321,#6322,#6323,#6324,#6325,#6326,#6327,#6328,#6329,#6330,#6331,#6332,
#6333,#6334,#6335,#6336,#6337,#6338,#6339,#6340,#6341,#6342,#6343,#6344,
#6345,#6346,#6347,#6348,#6349,#6350,#6351,#6352,#6353,#6354,#6355,#6356,
#6357,#6358,#6359,#6360,#6361,#6362,#6363,#6364,#6365,#6366,#6367,#6368,
#6369,#6370,#6371,#6372),.UNSPECIFIED.,.F.,.F.,(4,3,3,3,3,3,3,3,3,3,3,3,
3,3,3,3,3,3,3,3,3,3,3,3,3,3,3,3,3,3,3,3,3,3,3,3,3,3,3,3,3,3,3,3,3,3,3,3,
3,3,3,3,3,3,3,3,3,3,3,3,3,3,3,4),(7.39737634520917,7.5045643963064,7.61181522811714,
7.71924509232123,7.82677710957549,7.9345284980795,7.97264698981127,8.07816920580476,
8.18353281643407,8.28877282842226,8.39394707248085,8.49909163221331,8.60424254715742,
8.70950530751085,8.81483114798201,8.92033820552694,8.96922786353769,9.07474698125427,
9.18010750983919,9.28534447958757,9.39051570803975,9.49565728357388,9.60080525053349,
9.70606513833567,9.81138814522103,9.91689245928974,9.96580873726409,10.0713229311904,
10.1766784331034,10.2819102485201,10.3870762463538,10.4922125229135,10.5973551303977,
10.7026096036373,10.8079271565929,10.9134260129313,10.9623896109905,11.0679074212527,
11.1732665931826,11.278502139918,11.3836719049369,11.4888119787845,11.5939584079301,
11.6992167135617,11.8045381106151,11.9100407888698,11.9589704847169,12.0644875831435,
12.1698460407089,12.2750808729382,12.3802499237997,12.4853892849515,12.5905350039773,
12.6957926083051,12.8011133080767,12.9066153025981,12.9555513584433,13.0600577982311,
13.1644187171344,13.2686717663157,13.372878279919,13.4770515526011,13.5812931985024,
13.6805616523888),.UNSPECIFIED.);
#824=B_SPLINE_CURVE_WITH_KNOTS('',3,(#6377,#6378,#6379,#6380,#6381,#6382,
#6383,#6384,#6385,#6386,#6387),.UNSPECIFIED.,.F.,.F.,(4,1,1,1,1,1,1,1,4),
(-22.9420976703771,-22.9213600957074,-21.924779221981,-20.9281983482546,
-19.9316174745282,-18.9350366008018,-17.9384557270754,-16.941874853349,
-16.6589168227746),.UNSPECIFIED.);
#825=B_SPLINE_CURVE_WITH_KNOTS('',3,(#6388,#6389,#6390,#6391,#6392,#6393,
#6394,#6395,#6396,#6397,#6398,#6399,#6400,#6401,#6402,#6403,#6404,#6405,
#6406,#6407,#6408,#6409,#6410,#6411,#6412,#6413,#6414,#6415,#6416,#6417,
#6418,#6419,#6420,#6421,#6422,#6423,#6424,#6425,#6426,#6427,#6428,#6429,
#6430,#6431,#6432,#6433,#6434,#6435,#6436,#6437,#6438,#6439,#6440,#6441,
#6442,#6443,#6444,#6445,#6446,#6447,#6448,#6449,#6450,#6451,#6452,#6453,
#6454,#6455,#6456,#6457,#6458,#6459,#6460,#6461,#6462,#6463,#6464,#6465,
#6466,#6467,#6468,#6469,#6470,#6471,#6472,#6473,#6474,#6475,#6476,#6477,
#6478,#6479,#6480,#6481,#6482,#6483,#6484,#6485,#6486,#6487,#6488,#6489,
#6490,#6491,#6492,#6493,#6494,#6495,#6496,#6497,#6498,#6499,#6500,#6501,
#6502,#6503,#6504,#6505,#6506,#6507,#6508,#6509,#6510,#6511,#6512,#6513,
#6514,#6515,#6516,#6517,#6518,#6519,#6520,#6521,#6522,#6523,#6524,#6525,
#6526,#6527,#6528,#6529,#6530,#6531,#6532,#6533,#6534,#6535,#6536,#6537,
#6538,#6539,#6540,#6541,#6542,#6543,#6544,#6545,#6546,#6547,#6548,#6549,
#6550,#6551,#6552,#6553,#6554,#6555,#6556,#6557,#6558,#6559,#6560,#6561,
#6562,#6563,#6564,#6565,#6566,#6567,#6568,#6569,#6570,#6571,#6572,#6573,
#6574,#6575,#6576,#6577),.UNSPECIFIED.,.F.,.F.,(4,3,3,3,3,3,3,3,3,3,3,3,
3,3,3,3,3,3,3,3,3,3,3,3,3,3,3,3,3,3,3,3,3,3,3,3,3,3,3,3,3,3,3,3,3,3,3,3,
3,3,3,3,3,3,3,3,3,3,3,3,3,3,3,4),(13.6805616528234,13.8163469424965,13.9521322321697,
14.0576492724172,14.1630076667914,14.2682424286896,14.37341140482,14.4785506869449,
14.5836963227472,14.6889538380414,14.7942744453278,14.8997763429845,14.9487131058961,
15.0542300102651,15.1595882677422,15.2648228919211,15.369991729905,15.4751308736699,
15.5802763711125,15.6855337490015,15.790854219229,15.8963559818009,15.9452939796226,
16.0508108200795,16.1561690120437,16.2614035686587,16.3665723378434,16.4717114116778,
16.5768568381605,16.6821141440126,16.7874345414829,16.8929362309439,16.941874853349,
17.0473917665423,17.1527500324105,17.2579846642936,17.3631535095492,17.4682926601413,
17.5734381639533,17.6786955474717,17.7840160229135,17.889517790002,17.9384557270754,
18.043972620432,18.149330866254,18.2545654778811,18.3597343027627,18.4648734328942,
18.5700189161904,18.6752762792507,18.7805967342379,18.8860984810917,18.9350366008018,
19.0405534775837,19.1459117066389,19.251146301295,19.3563151090886,19.4614542220405,
19.5665996880905,19.6718570339203,19.7771774716607,19.8826792014214,19.9316174745282,
19.9637469595683),.UNSPECIFIED.);
#826=B_SPLINE_CURVE_WITH_KNOTS('',3,(#6582,#6583,#6584,#6585,#6586,#6587,
#6588,#6589,#6590,#6591,#6592,#6593,#6594,#6595,#6596,#6597,#6598,#6599,
#6600,#6601,#6602,#6603,#6604,#6605,#6606,#6607,#6608,#6609,#6610,#6611,
#6612,#6613,#6614,#6615,#6616,#6617,#6618,#6619,#6620,#6621,#6622,#6623,
#6624,#6625,#6626,#6627,#6628,#6629,#6630,#6631,#6632,#6633,#6634,#6635,
#6636,#6637,#6638,#6639,#6640,#6641,#6642,#6643,#6644,#6645,#6646,#6647,
#6648,#6649,#6650,#6651,#6652,#6653,#6654,#6655,#6656,#6657,#6658,#6659,
#6660,#6661,#6662,#6663,#6664,#6665,#6666,#6667,#6668,#6669,#6670,#6671,
#6672,#6673,#6674,#6675,#6676,#6677,#6678,#6679,#6680,#6681,#6682,#6683,
#6684,#6685,#6686,#6687,#6688,#6689,#6690,#6691,#6692,#6693,#6694,#6695,
#6696,#6697,#6698,#6699,#6700,#6701,#6702,#6703,#6704,#6705,#6706,#6707,
#6708,#6709,#6710,#6711,#6712,#6713,#6714,#6715,#6716,#6717,#6718,#6719,
#6720,#6721,#6722,#6723,#6724,#6725,#6726,#6727,#6728,#6729,#6730,#6731,
#6732,#6733,#6734,#6735,#6736,#6737,#6738,#6739,#6740,#6741,#6742,#6743,
#6744,#6745,#6746,#6747,#6748,#6749,#6750,#6751,#6752,#6753,#6754,#6755,
#6756,#6757,#6758,#6759,#6760,#6761,#6762,#6763,#6764,#6765,#6766,#6767,
#6768,#6769,#6770,#6771),.UNSPECIFIED.,.F.,.F.,(4,3,3,3,3,3,3,3,3,3,3,3,
3,3,3,3,3,3,3,3,3,3,3,3,3,3,3,3,3,3,3,3,3,3,3,3,3,3,3,3,3,3,3,3,3,3,3,3,
3,3,3,3,3,3,3,3,3,3,3,3,3,3,3,4),(-29.2252829771425,-29.1019668884045,-28.9772671757159,
-28.9008453380659,-28.7953311638247,-28.6899756819199,-28.5847438868928,
-28.4795779096734,-28.3744416539219,-28.269299067409,-28.1640446152449,
-28.0587270834549,-27.953228248201,-27.9042644643395,-27.7987466448287,
-27.6933874635456,-27.5881519073482,-27.4829821328055,-27.3778420493867,
-27.2726956106372,-27.1674372954176,-27.0621158887715,-26.956613201017,
-26.9076835906131,-26.8021664914534,-26.696808033114,-26.5915732000532,
-26.486404148325,-26.3812647862725,-26.2761190663134,-26.1708614610086,
-26.0655407602334,-25.9600387646784,-25.9111027168866,-25.8055861967743,
-25.7002283306547,-25.5949941064194,-25.4898256734777,-25.3846869392369,
-25.2795418551893,-25.1742848937338,-25.0689648422825,-24.9634634977247,
-24.9145218431602,-24.8090048011679,-24.7036464050276,-24.5984116413407,
-24.4932426634085,-24.3881033794714,-24.2829577418493,-24.1777002247363,
-24.0723796156288,-23.966877716167,-23.9179409694338,-23.8127945908852,
-23.7039574758217,-23.5990948008806,-23.494295154551,-23.3895219001087,
-23.2847384419461,-23.1798422596678,-23.074878461885,-22.9697413145948,
-22.9420976703771),.UNSPECIFIED.);
#827=B_SPLINE_CURVE_WITH_KNOTS('',3,(#6772,#6773,#6774,#6775,#6776,#6777,
#6778,#6779,#6780,#6781),.UNSPECIFIED.,.F.,.F.,(4,1,1,1,1,1,1,4),(19.9637512898265,
20.9281983482546,21.924779221981,22.9213600957074,23.9179409694338,24.9145218431602,
25.9111027168866,26.2469251046285),.UNSPECIFIED.);
#828=B_SPLINE_CURVE_WITH_KNOTS('',3,(#6786,#6787,#6788,#6789,#6790,#6791,
#6792,#6793,#6794,#6795,#6796,#6797,#6798,#6799,#6800,#6801,#6802,#6803,
#6804,#6805,#6806,#6807,#6808,#6809,#6810,#6811,#6812,#6813,#6814,#6815,
#6816,#6817,#6818,#6819,#6820,#6821,#6822,#6823,#6824,#6825,#6826,#6827,
#6828,#6829,#6830,#6831,#6832,#6833,#6834,#6835,#6836,#6837,#6838,#6839,
#6840,#6841,#6842,#6843,#6844,#6845,#6846,#6847,#6848,#6849,#6850,#6851,
#6852,#6853,#6854,#6855,#6856,#6857,#6858,#6859,#6860,#6861,#6862,#6863,
#6864,#6865,#6866,#6867,#6868,#6869,#6870,#6871,#6872,#6873,#6874,#6875,
#6876,#6877,#6878,#6879,#6880,#6881,#6882,#6883,#6884,#6885,#6886,#6887,
#6888,#6889,#6890,#6891,#6892,#6893,#6894,#6895,#6896,#6897,#6898,#6899,
#6900,#6901,#6902,#6903,#6904,#6905,#6906,#6907,#6908,#6909,#6910,#6911,
#6912,#6913,#6914,#6915,#6916,#6917,#6918,#6919,#6920,#6921,#6922,#6923,
#6924,#6925,#6926,#6927,#6928,#6929,#6930,#6931,#6932,#6933,#6934,#6935,
#6936,#6937,#6938,#6939,#6940,#6941,#6942,#6943,#6944,#6945,#6946,#6947,
#6948,#6949,#6950,#6951,#6952,#6953,#6954,#6955,#6956,#6957,#6958,#6959,
#6960,#6961,#6962,#6963,#6964,#6965,#6966,#6967,#6968,#6969,#6970,#6971,
#6972,#6973,#6974,#6975),.UNSPECIFIED.,.F.,.F.,(4,3,3,3,3,3,3,3,3,3,3,3,
3,3,3,3,3,3,3,3,3,3,3,3,3,3,3,3,3,3,3,3,3,3,3,3,3,3,3,3,3,3,3,3,3,3,3,3,
3,3,3,3,3,3,3,3,3,3,3,3,3,3,3,4),(-35.5084682847362,-35.4023595064501,-35.2962353664595,
-35.1899767723763,-35.0836517048971,-34.9771072128198,-34.8803305804243,
-34.774950120342,-34.6697303251661,-34.5646364761803,-34.4596097707505,
-34.3546139040873,-34.2496126168141,-34.1444998826447,-34.0393245183892,
-33.9339670573159,-33.8837497066979,-33.7782042662091,-33.6728173464079,
-33.5675540178141,-33.4623564669828,-33.357188646819,-33.2520145543265,
-33.1467289026187,-33.0413803014023,-32.935850924157,-32.8871688329715,
-32.7816310902558,-32.6762515117445,-32.570994956414,-32.4658038211252,
-32.3606420477127,-32.2554736217244,-32.1501930189174,-32.0448491206367,
-31.9393238610627,-31.8905879592451,-31.7850905501634,-31.6797520943826,
-31.5745376278472,-31.4693891567627,-31.3642705581269,-31.2591457532205,
-31.1539091496212,-31.0486095307009,-30.9431285201142,-30.8940070855187,
-30.7884848231671,-30.6831211656924,-30.5778811063686,-30.4727068146982,
-30.367562207151,-30.2624112442611,-30.1571484360919,-30.0518225478098,
-29.9463154429618,-29.8974262117923,-29.7921249664941,-29.6869771514366,
-29.5819461862507,-29.476987732131,-29.3720711679722,-29.2671322858929,
-29.2252829775566),.UNSPECIFIED.);
#829=B_SPLINE_CURVE_WITH_KNOTS('',3,(#6976,#6977,#6978,#6979,#6980,#6981,
#6982,#6983,#6984,#6985,#6986,#6987,#6988,#6989,#6990,#6991,#6992,#6993,
#6994,#6995,#6996,#6997,#6998,#6999,#7000,#7001,#7002,#7003,#7004,#7005,
#7006,#7007,#7008,#7009,#7010,#7011,#7012,#7013,#7014,#7015,#7016,#7017,
#7018,#7019,#7020,#7021,#7022,#7023,#7024,#7025,#7026,#7027,#7028,#7029,
#7030,#7031,#7032,#7033,#7034,#7035,#7036,#7037,#7038,#7039,#7040,#7041,
#7042,#7043,#7044,#7045,#7046,#7047,#7048,#7049,#7050,#7051,#7052,#7053,
#7054,#7055,#7056,#7057,#7058,#7059,#7060,#7061,#7062,#7063,#7064,#7065,
#7066,#7067,#7068,#7069,#7070,#7071,#7072,#7073,#7074,#7075,#7076,#7077,
#7078,#7079,#7080,#7081,#7082,#7083,#7084,#7085,#7086,#7087,#7088,#7089,
#7090,#7091,#7092,#7093,#7094,#7095,#7096,#7097,#7098,#7099,#7100,#7101,
#7102,#7103,#7104,#7105,#7106,#7107,#7108,#7109,#7110,#7111,#7112,#7113,
#7114,#7115,#7116,#7117,#7118,#7119,#7120,#7121,#7122,#7123,#7124,#7125,
#7126,#7127,#7128,#7129,#7130,#7131,#7132,#7133,#7134,#7135,#7136,#7137,
#7138,#7139,#7140,#7141,#7142,#7143,#7144,#7145,#7146,#7147,#7148,#7149,
#7150,#7151,#7152,#7153,#7154,#7155,#7156,#7157,#7158,#7159,#7160,#7161,
#7162,#7163,#7164,#7165),.UNSPECIFIED.,.F.,.F.,(4,3,3,3,3,3,3,3,3,3,3,3,
3,3,3,3,3,3,3,3,3,3,3,3,3,3,3,3,3,3,3,3,3,3,3,3,3,3,3,3,3,3,3,3,3,3,3,3,
3,3,3,3,3,3,3,3,3,3,3,3,3,3,3,4),(26.2469322667479,26.3520739127527,26.457200702523,
26.5623485411171,26.6676237508216,26.7729747238681,26.8785103872483,26.9076835906131,
27.0132014116089,27.118560591826,27.2237961432062,27.328965910607,27.4341059845773,
27.5392524115879,27.6445107117001,27.749832101293,27.855334769187,27.9042644643395,
28.009778477704,28.115133840206,28.2203655774866,28.325531535249,28.4306678097399,
28.5358104531352,28.6410650192125,28.7463826976559,28.8518817282747,28.9008453380659,
29.0063647936613,29.1117255831179,29.2169626990727,29.3221340024984,29.4272755818899,
29.532423481632,29.6376831956915,29.7430059677345,29.8485099556621,29.8974262117923,
30.0029483903628,30.1083119720987,30.2135519678938,30.318726203649,30.4238707629551,
30.5290216853453,30.6342844649434,30.7396103314267,30.8451174250954,30.8940070855187,
30.9995034308467,31.1048410912434,31.2100551614917,31.31520348413,31.4203221815892,
31.5254473322799,31.6306846511216,31.7359851973197,31.8414674509995,31.8905879592451,
31.9966053193322,32.1024616306616,32.2093756164781,32.315013108761,32.4225653413443,
32.5301175739275),.UNSPECIFIED.);
#830=B_SPLINE_CURVE_WITH_KNOTS('',3,(#7168,#7169,#7170,#7171,#7172,#7173,
#7174,#7175,#7176,#7177,#7178,#7179,#7180,#7181,#7182,#7183,#7184,#7185,
#7186,#7187,#7188,#7189,#7190,#7191,#7192,#7193,#7194,#7195,#7196,#7197,
#7198,#7199,#7200,#7201,#7202,#7203,#7204,#7205,#7206,#7207,#7208,#7209,
#7210,#7211,#7212,#7213,#7214,#7215,#7216,#7217,#7218,#7219,#7220,#7221,
#7222,#7223,#7224,#7225,#7226,#7227,#7228,#7229,#7230,#7231,#7232,#7233,
#7234,#7235,#7236,#7237,#7238,#7239,#7240,#7241,#7242,#7243,#7244,#7245,
#7246,#7247,#7248,#7249,#7250,#7251,#7252,#7253,#7254,#7255,#7256,#7257,
#7258,#7259,#7260,#7261,#7262,#7263,#7264,#7265,#7266,#7267,#7268,#7269,
#7270,#7271,#7272,#7273,#7274,#7275,#7276,#7277,#7278,#7279,#7280,#7281,
#7282,#7283,#7284,#7285,#7286,#7287,#7288,#7289,#7290,#7291,#7292,#7293,
#7294),.UNSPECIFIED.,.F.,.F.,(4,3,3,3,3,3,3,3,3,3,3,3,3,3,3,3,3,3,3,3,3,
3,3,3,3,3,3,3,3,3,3,3,3,3,3,3,3,3,3,3,3,3,4),(32.5301175743904,32.6499243852403,
32.7707627025496,32.8871688329715,32.9927129802535,33.0980988488266,33.2033614876022,
33.3085585732964,33.4137261529851,33.5189002298821,33.6241862045267,33.7295353225629,
33.8350655085771,33.8837497066979,33.9891233821121,34.0943380597535,34.1994292723219,
34.3044548813996,34.4094511884809,34.5144544512916,34.6195714611784,34.7247524196896,
34.8301174455497,34.8803305804243,34.9860472709756,35.0916046934767,35.1970366054674,
35.3024014441107,35.4077350088511,35.5130730534988,35.6185188580414,35.7240256643669,
35.8297086352625,35.8769114541507,35.9814256971422,36.085764885428,36.1900065327749,
36.2941881420584,36.3983471341029,36.5025900738691,36.6068728780943,36.7113371001607,
36.8011443739907),.UNSPECIFIED.);
#831=B_SPLINE_CURVE_WITH_KNOTS('',3,(#7297,#7298,#7299,#7300,#7301,#7302,
#7303),.UNSPECIFIED.,.F.,.F.,(4,1,1,1,4),(-38.86665407533,-37.8700732016036,
-36.8734923278771,-35.8769114541507,-35.5084758780373),.UNSPECIFIED.);
#832=B_SPLINE_CURVE_WITH_KNOTS('',3,(#7306,#7307,#7308,#7309,#7310,#7311,
#7312,#7313,#7314,#7315,#7316,#7317,#7318,#7319,#7320,#7321,#7322,#7323,
#7324,#7325,#7326,#7327,#7328,#7329,#7330,#7331,#7332,#7333,#7334,#7335,
#7336,#7337,#7338,#7339,#7340,#7341,#7342),.UNSPECIFIED.,.F.,.F.,(4,3,3,
3,3,3,3,3,3,3,3,3,4),(47.1238898038469,47.2495729833432,47.3762357179408,
47.4923329732614,47.6078590787388,47.7183089200037,47.8286551120703,47.9389421371105,
48.0492143835049,48.1595854549815,48.2700151013785,48.3806268044217,48.4165418170808),
 .UNSPECIFIED.);
#833=B_SPLINE_CURVE_WITH_KNOTS('',3,(#7345,#7346,#7347,#7348,#7349,#7350),
 .UNSPECIFIED.,.F.,.F.,(4,2,4),(9.70317678897598E-6,0.00416850045810854,
0.00832730327464804),.UNSPECIFIED.);
#834=B_SPLINE_CURVE_WITH_KNOTS('',3,(#7519,#7520,#7521,#7522,#7523,#7524,
#7525,#7526,#7527,#7528,#7529,#7530,#7531,#7532,#7533,#7534,#7535,#7536,
#7537,#7538,#7539,#7540,#7541,#7542,#7543,#7544,#7545,#7546,#7547,#7548,
#7549,#7550,#7551,#7552,#7553,#7554,#7555,#7556,#7557,#7558,#7559,#7560,
#7561,#7562,#7563,#7564,#7565,#7566,#7567,#7568,#7569,#7570,#7571,#7572,
#7573,#7574,#7575,#7576,#7577,#7578,#7579,#7580,#7581,#7582,#7583,#7584,
#7585,#7586,#7587,#7588,#7589,#7590,#7591,#7592,#7593,#7594,#7595,#7596,
#7597,#7598,#7599,#7600,#7601,#7602,#7603,#7604,#7605,#7606),
 .UNSPECIFIED.,.F.,.F.,(4,3,3,3,3,3,3,3,3,3,3,3,3,3,3,3,3,3,3,3,3,3,3,3,
3,3,3,3,3,4),(0.,0.0141071418350746,0.0355442788990485,0.0572656760919848,
0.0669720866841882,0.0731473068623763,0.0768712322010848,0.097962135648359,
0.118760026435029,0.139128689171555,0.144047130563164,0.148652874159979,
0.168817015633453,0.188376963157815,0.19974270647635,0.210158636009444,
0.214504663218229,0.217541294053797,0.237154834658274,0.256934379130968,
0.270710750322308,0.279046676847462,0.284344207394495,0.303389528646404,
0.31873922745522,0.324227329017253,0.328196248006345,0.346653672870525,
0.365111097734705,0.366397579005847),.UNSPECIFIED.);
#835=B_SPLINE_CURVE_WITH_KNOTS('',3,(#7607,#7608,#7609,#7610,#7611,#7612,
#7613,#7614,#7615,#7616,#7617,#7618,#7619,#7620,#7621,#7622,#7623,#7624,
#7625,#7626,#7627,#7628,#7629,#7630,#7631,#7632,#7633,#7634,#7635,#7636,
#7637,#7638,#7639,#7640,#7641,#7642,#7643,#7644,#7645,#7646,#7647,#7648,
#7649,#7650,#7651,#7652,#7653,#7654,#7655,#7656,#7657,#7658,#7659,#7660,
#7661,#7662,#7663,#7664,#7665,#7666,#7667,#7668,#7669,#7670,#7671,#7672,
#7673,#7674,#7675,#7676,#7677,#7678,#7679,#7680,#7681,#7682,#7683,#7684,
#7685,#7686,#7687,#7688,#7689,#7690,#7691,#7692,#7693,#7694),
 .UNSPECIFIED.,.F.,.F.,(4,3,3,3,3,3,3,3,3,3,3,3,3,3,3,3,3,3,3,3,3,3,3,3,
3,3,3,3,3,4),(0.,0.0113475426890351,0.0295973948769154,0.0478472470647956,
0.056029692194114,0.0601609064742412,0.0640260637796794,0.0829599659548612,
0.102409502743582,0.12142565969715,0.125492936129605,0.128447152844756,
0.148489790019264,0.168489720575875,0.178766369133891,0.190382802806189,
0.193958991934283,0.213737709639448,0.233952453150079,0.254598727957293,
0.259921705844119,0.263839735837504,0.267527540816782,0.288775631129183,
0.3076511551242,0.313183531178787,0.317664298570661,0.339328410842523,0.360810180213187,
0.364629307890663),.UNSPECIFIED.);
#836=B_SPLINE_CURVE_WITH_KNOTS('',3,(#7863,#7864,#7865,#7866,#7867,#7868,
#7869,#7870,#7871,#7872,#7873,#7874,#7875,#7876,#7877,#7878,#7879,#7880,
#7881,#7882,#7883,#7884,#7885,#7886,#7887,#7888,#7889,#7890,#7891,#7892,
#7893,#7894,#7895,#7896,#7897,#7898,#7899,#7900,#7901,#7902,#7903,#7904,
#7905,#7906,#7907,#7908,#7909,#7910,#7911,#7912,#7913,#7914,#7915,#7916,
#7917,#7918,#7919,#7920,#7921,#7922,#7923,#7924,#7925,#7926,#7927,#7928,
#7929,#7930,#7931,#7932,#7933,#7934,#7935,#7936,#7937,#7938,#7939,#7940,
#7941,#7942,#7943,#7944,#7945,#7946,#7947,#7948,#7949,#7950),
 .UNSPECIFIED.,.F.,.F.,(4,3,3,3,3,3,3,3,3,3,3,3,3,3,3,3,3,3,3,3,3,3,3,3,
3,3,3,3,3,4),(0.,0.0113475426890348,0.0291670043826812,0.0475729265912865,
0.0560296567510774,0.0601608189470318,0.0640260370135678,0.0829599116450913,
0.1024094459103,0.121425612309687,0.125492777420358,0.128446963999971,0.148489595673194,
0.168489527887108,0.178766369133891,0.19038280280619,0.196167693616744,
0.215997966192077,0.236257447265082,0.256915792055175,0.259921709458412,
0.263839753802059,0.267527548188019,0.288775627558559,0.307651148858093,
0.313183536190041,0.317664301193788,0.339328429311912,0.360810221499639,
0.364629307890676),.UNSPECIFIED.);
#837=B_SPLINE_CURVE_WITH_KNOTS('',3,(#7951,#7952,#7953,#7954,#7955,#7956,
#7957,#7958,#7959,#7960,#7961,#7962,#7963,#7964,#7965,#7966,#7967,#7968,
#7969,#7970,#7971,#7972,#7973,#7974,#7975,#7976,#7977,#7978,#7979,#7980,
#7981,#7982,#7983,#7984,#7985,#7986,#7987,#7988,#7989,#7990,#7991,#7992,
#7993,#7994,#7995,#7996,#7997,#7998,#7999,#8000,#8001,#8002,#8003,#8004,
#8005,#8006,#8007,#8008,#8009,#8010,#8011,#8012,#8013,#8014,#8015,#8016,
#8017,#8018,#8019,#8020,#8021,#8022,#8023,#8024,#8025,#8026,#8027,#8028,
#8029,#8030,#8031,#8032,#8033,#8034,#8035),.UNSPECIFIED.,.F.,.F.,(4,3,3,
3,3,3,3,3,3,3,3,3,3,3,3,3,3,3,3,3,3,3,3,3,3,3,3,3,4),(0.,0.0141071418350769,
0.0355831078562044,0.0572869708038222,0.0731472545817825,0.07687123101439,
0.0979621340421377,0.118760002281852,0.139128677516317,0.144047115677256,
0.148652871053239,0.168816990654727,0.1883768924813,0.199742706476349,0.210158636009442,
0.214504668205586,0.217541304162528,0.237140058799154,0.257539855958027,
0.272839703827182,0.279653079547202,0.284485042082695,0.303528865961174,
0.318739247434647,0.32422724443456,0.328196234497253,0.34665369295304,0.365111151408828,
0.366397579005838),.UNSPECIFIED.);
#838=B_SPLINE_CURVE_WITH_KNOTS('',3,(#8081,#8082,#8083,#8084,#8085,#8086,
#8087,#8088,#8089,#8090,#8091,#8092,#8093,#8094,#8095,#8096,#8097,#8098,
#8099,#8100,#8101,#8102,#8103,#8104,#8105,#8106,#8107,#8108,#8109,#8110,
#8111,#8112,#8113,#8114,#8115,#8116,#8117,#8118,#8119,#8120,#8121,#8122,
#8123,#8124,#8125,#8126,#8127,#8128,#8129,#8130,#8131,#8132,#8133,#8134,
#8135,#8136,#8137,#8138,#8139,#8140,#8141,#8142,#8143,#8144,#8145,#8146,
#8147,#8148,#8149,#8150,#8151,#8152,#8153,#8154,#8155,#8156,#8157,#8158,
#8159,#8160,#8161,#8162,#8163,#8164,#8165,#8166,#8167,#8168,#8169,#8170,
#8171,#8172,#8173,#8174,#8175,#8176,#8177,#8178,#8179,#8180,#8181,#8182,
#8183,#8184,#8185,#8186,#8187,#8188,#8189,#8190,#8191,#8192,#8193,#8194,
#8195,#8196,#8197,#8198,#8199,#8200,#8201,#8202,#8203,#8204,#8205,#8206,
#8207,#8208,#8209,#8210,#8211,#8212,#8213,#8214,#8215,#8216,#8217,#8218,
#8219,#8220,#8221,#8222,#8223,#8224,#8225,#8226,#8227,#8228),
 .UNSPECIFIED.,.F.,.F.,(4,3,3,3,3,3,3,3,3,3,3,3,3,3,3,3,3,3,3,3,3,3,3,3,
3,3,3,3,3,3,3,3,3,3,3,3,3,3,3,3,3,3,3,3,3,3,3,3,3,4),(10.3761213044057,
10.4916473343449,10.6020836926387,10.7124212898676,10.8227045964878,10.932977995856,
11.0433574182079,11.153799603579,11.2644299007573,11.300329543919,11.412228455198,
11.5239351693938,11.6355347254555,11.7470696766159,11.8585824834668,11.9701986021098,
12.0818627300226,12.1937439049619,12.2969104176454,12.4084748637133,12.5198380200048,
12.6310887295725,12.7422701582708,12.8534253726942,12.9646803676604,13.0759808484134,
13.1874988487555,13.2934912913718,13.4052296275761,13.5167698094669,13.6281993328827,
13.7395610570682,13.8508977444198,13.9623346136356,14.07381749289,14.185516391903,
14.2900721650982,14.4018025327098,14.5133353791798,14.6247579576194,14.7361131396909,
14.8474437006735,14.9588751530412,15.0703529943081,15.1820475712269,15.2866530388247,
15.4088138904717,15.5306080160374,15.6518307149658,15.7079632679489),
 .UNSPECIFIED.);
#839=B_SPLINE_CURVE_WITH_KNOTS('',3,(#8231,#8232,#8233,#8234,#8235,#8236,
#8237,#8238,#8239,#8240,#8241,#8242,#8243,#8244,#8245,#8246,#8247,#8248,
#8249,#8250,#8251,#8252,#8253,#8254,#8255,#8256,#8257,#8258,#8259,#8260,
#8261,#8262,#8263,#8264,#8265,#8266,#8267,#8268,#8269,#8270,#8271,#8272,
#8273,#8274,#8275,#8276,#8277,#8278,#8279,#8280,#8281,#8282,#8283,#8284,
#8285,#8286,#8287,#8288,#8289,#8290,#8291,#8292,#8293,#8294,#8295,#8296,
#8297,#8298,#8299,#8300,#8301,#8302,#8303,#8304,#8305,#8306,#8307,#8308,
#8309,#8310,#8311,#8312,#8313,#8314,#8315,#8316,#8317,#8318,#8319,#8320,
#8321,#8322,#8323,#8324,#8325,#8326,#8327,#8328,#8329,#8330,#8331,#8332,
#8333,#8334,#8335,#8336,#8337,#8338,#8339,#8340,#8341,#8342),
 .UNSPECIFIED.,.F.,.F.,(4,3,3,3,3,3,3,3,3,3,3,3,3,3,3,3,3,3,3,3,3,3,3,3,
3,3,3,3,3,3,3,3,3,3,3,3,3,4),(11.6154215191107,11.7297194433804,11.8439615074736,
11.9581751212632,12.0723949424661,12.1866556269815,12.3010886611519,12.4156103002373,
12.5303749287406,12.6120023928371,12.722600396268,12.8333482550549,12.9435980012706,
13.0537674854308,13.1639012473881,13.275071752182,13.3853379846654,13.4969606256144,
13.6085832665635,13.7204465169992,13.8321110831576,13.9436645730413,14.0551496181406,
14.16660875264,14.2781656624489,14.3897674585362,14.5015817699047,14.6051641402899,
14.7170632550792,14.8287701821625,14.9403699566644,15.0519051314419,15.1634181667176,
15.2750345195736,15.3866988852361,15.4985803008964,15.6017450140163,15.7079632679489),
 .UNSPECIFIED.);
#840=B_SPLINE_CURVE_WITH_KNOTS('',3,(#8347,#8348,#8349,#8350,#8351,#8352,
#8353,#8354,#8355,#8356),.UNSPECIFIED.,.F.,.F.,(4,1,1,1,1,1,1,4),(15.7079632679489,
16.2832339125511,17.2798147862775,18.2763956600039,19.2729765337303,20.2695574074567,
21.2661382811831,21.9911485751285),.UNSPECIFIED.);
#841=B_SPLINE_CURVE_WITH_KNOTS('',3,(#8357,#8358,#8359,#8360,#8361,#8362,
#8363,#8364,#8365,#8366),.UNSPECIFIED.,.F.,.F.,(4,1,1,1,1,1,1,4),(15.7079720007471,
16.5983258877427,17.5949067614691,18.5914876351955,19.5880685089219,20.5846493826483,
21.5812302563748,21.9911424371547),.UNSPECIFIED.);
#842=B_SPLINE_CURVE_WITH_KNOTS('',3,(#8371,#8372,#8373,#8374,#8375,#8376,
#8377,#8378,#8379,#8380,#8381,#8382,#8383,#8384,#8385,#8386,#8387,#8388,
#8389,#8390,#8391,#8392,#8393,#8394,#8395,#8396,#8397,#8398,#8399,#8400,
#8401,#8402,#8403,#8404,#8405,#8406,#8407,#8408,#8409,#8410,#8411,#8412,
#8413,#8414,#8415,#8416,#8417,#8418,#8419,#8420,#8421,#8422,#8423,#8424,
#8425,#8426,#8427,#8428,#8429,#8430,#8431,#8432,#8433,#8434,#8435,#8436,
#8437,#8438,#8439,#8440,#8441,#8442,#8443,#8444,#8445,#8446,#8447,#8448,
#8449,#8450,#8451,#8452,#8453,#8454,#8455,#8456,#8457,#8458,#8459,#8460,
#8461,#8462,#8463,#8464,#8465,#8466,#8467,#8468,#8469,#8470,#8471,#8472,
#8473,#8474,#8475,#8476,#8477,#8478,#8479,#8480,#8481,#8482,#8483,#8484,
#8485,#8486,#8487,#8488,#8489,#8490,#8491,#8492,#8493,#8494,#8495,#8496,
#8497,#8498,#8499,#8500,#8501,#8502,#8503,#8504,#8505,#8506,#8507,#8508,
#8509,#8510,#8511,#8512,#8513,#8514,#8515,#8516,#8517,#8518,#8519,#8520,
#8521,#8522,#8523,#8524,#8525,#8526,#8527,#8528,#8529,#8530,#8531,#8532,
#8533,#8534,#8535,#8536,#8537,#8538,#8539,#8540,#8541,#8542),
 .UNSPECIFIED.,.F.,.F.,(4,3,3,3,3,3,3,3,3,3,3,3,3,3,3,3,3,3,3,3,3,3,3,3,
3,3,3,3,3,3,3,3,3,3,3,3,3,3,3,3,3,3,3,3,3,3,3,3,3,3,3,3,3,3,3,3,3,4),(21.9911485751285,
22.1309179503358,22.2627191549095,22.374427659155,22.4859378873352,22.5973374041085,
22.708669121392,22.8199758541662,22.9313830961258,23.0428364782555,23.154506491853,
23.2593000286359,23.3710083890299,23.4825184720439,23.5939178429524,23.7052494139272,
23.8165560002028,23.9279630965552,24.0394163333242,24.1510862038984,24.2558809023623,
24.3675891950941,24.479099207913,24.5904985071345,24.7018300050549,24.8131365170312,
24.9245435377139,25.0359966979394,25.1476664914795,25.2524617760888,25.3641701458249,
25.4756802374145,25.5870796164264,25.698411195018,25.8097177884088,25.9211248910232,
26.0325781335982,26.1442480091204,26.2490426498152,26.3607509985506,26.4722610688441,
26.5836604263951,26.6949919833986,26.8062985551115,26.9177056360823,27.0291588569969,
27.1408287111152,27.2456235235416,27.3573318547298,27.4688419071979,27.5802412467662,
27.69157278566,27.8028793391663,27.9142864019217,28.0257396045859,28.1374094406313,
28.242204397268,28.2743338823081),.UNSPECIFIED.);
#843=B_SPLINE_CURVE_WITH_KNOTS('',3,(#8543,#8544,#8545,#8546,#8547,#8548,
#8549,#8550,#8551,#8552,#8553,#8554,#8555,#8556,#8557,#8558,#8559,#8560,
#8561,#8562,#8563,#8564,#8565,#8566,#8567,#8568,#8569,#8570,#8571,#8572,
#8573,#8574,#8575,#8576,#8577,#8578,#8579,#8580,#8581,#8582,#8583,#8584,
#8585,#8586,#8587,#8588,#8589,#8590,#8591,#8592,#8593,#8594,#8595,#8596,
#8597,#8598,#8599,#8600,#8601,#8602,#8603,#8604,#8605,#8606,#8607,#8608,
#8609,#8610,#8611,#8612,#8613,#8614,#8615,#8616,#8617,#8618,#8619,#8620,
#8621,#8622,#8623,#8624,#8625,#8626,#8627,#8628,#8629,#8630,#8631,#8632,
#8633,#8634,#8635,#8636,#8637,#8638,#8639,#8640,#8641,#8642,#8643,#8644,
#8645,#8646,#8647,#8648,#8649,#8650,#8651,#8652,#8653,#8654,#8655,#8656,
#8657,#8658,#8659,#8660,#8661,#8662,#8663,#8664,#8665,#8666,#8667,#8668,
#8669,#8670,#8671,#8672,#8673,#8674,#8675,#8676,#8677,#8678,#8679,#8680),
 .UNSPECIFIED.,.F.,.F.,(4,2,2,2,2,2,2,2,2,2,2,2,2,2,2,2,2,2,2,2,2,2,2,2,
2,2,2,2,2,2,2,2,2,2,2,2,2,2,2,2,2,2,2,2,2,2,2,2,2,2,2,2,2,2,2,2,2,2,2,2,
2,2,2,2,2,2,2,2,4),(-1.96132285312146,-1.95620459237246,-1.95112567209526,
-1.94407886899802,-1.93468750571801,-1.89450594179228,-1.87724383315922,
-1.87143625996712,-1.86694093922326,-1.86026887903385,-1.83789122879064,
-1.81618308493092,-1.80542210271837,-1.79582903054646,-1.78805500328292,
-1.77835298749607,-1.74007387301098,-1.72193674407494,-1.71607184312288,
-1.71158118248237,-1.70498599765907,-1.67367749172583,-1.6513893744781,
-1.64126210789743,-1.63347268309289,-1.62422921768041,-1.58433775584925,
-1.56641843112916,-1.56056655351619,-1.55607455783141,-1.54946145498585,
-1.52436713357013,-1.50423730261349,-1.48998255539148,-1.48165848150001,
-1.47358902532616,-1.46108025679645,-1.4282076135,-1.41086123200036,-1.40504615407646,
-1.40054983866323,-1.39388294241964,-1.37115429218779,-1.3496453589913,
-1.3389271195264,-1.32935873731568,-1.32158243299074,-1.31184947095414,
-1.27375464582685,-1.25550601013682,-1.24963320639476,-1.24514198355881,
-1.23855416260086,-1.20717250984067,-1.18487207018713,-1.17476070399432,
-1.16696998774258,-1.15771014629021,-1.11807295920766,-1.0999546380503,
-1.09408914514634,-1.0895968159218,-1.0840808169788,-1.05331978181438,-1.02917947127776,
-1.01912619633388,-1.01133793422825,-1.00203406270535,-0.980953657893252),
 .UNSPECIFIED.);
#844=B_SPLINE_CURVE_WITH_KNOTS('',3,(#8685,#8686,#8687,#8688,#8689,#8690,
#8691,#8692,#8693,#8694,#8695,#8696,#8697,#8698,#8699,#8700,#8701,#8702,
#8703,#8704,#8705,#8706,#8707,#8708,#8709,#8710,#8711,#8712,#8713,#8714,
#8715,#8716,#8717,#8718,#8719,#8720,#8721,#8722,#8723,#8724,#8725,#8726,
#8727,#8728,#8729,#8730,#8731,#8732,#8733,#8734,#8735,#8736,#8737,#8738,
#8739,#8740,#8741,#8742,#8743,#8744,#8745,#8746,#8747,#8748,#8749,#8750,
#8751,#8752,#8753,#8754,#8755,#8756,#8757,#8758,#8759,#8760,#8761,#8762,
#8763,#8764,#8765,#8766,#8767,#8768,#8769,#8770,#8771,#8772,#8773,#8774,
#8775,#8776,#8777,#8778,#8779,#8780,#8781,#8782,#8783,#8784,#8785,#8786,
#8787,#8788,#8789,#8790,#8791,#8792,#8793,#8794,#8795,#8796,#8797,#8798,
#8799,#8800,#8801,#8802,#8803,#8804,#8805,#8806,#8807,#8808,#8809,#8810,
#8811,#8812,#8813,#8814,#8815,#8816,#8817,#8818,#8819,#8820,#8821,#8822,
#8823,#8824,#8825,#8826,#8827,#8828,#8829,#8830,#8831,#8832,#8833,#8834,
#8835,#8836,#8837,#8838,#8839,#8840,#8841,#8842,#8843,#8844,#8845,#8846,
#8847,#8848,#8849,#8850,#8851,#8852,#8853,#8854,#8855,#8856),
 .UNSPECIFIED.,.F.,.F.,(4,3,3,3,3,3,3,3,3,3,3,3,3,3,3,3,3,3,3,3,3,3,3,3,
3,3,3,3,3,3,3,3,3,3,3,3,3,3,3,3,3,3,3,3,3,3,3,3,3,3,3,3,3,3,3,3,3,4),(28.2743338828609,
28.3854499463252,28.4963720118464,28.6071867805496,28.717938100074,28.8286697232354,
28.9395040413308,29.0503910293875,29.1614837232968,29.2387852709944,29.3504936415298,
29.4620037336245,29.5734031129625,29.6847346917019,29.7960412850625,29.9074483873677,
30.0189016294807,30.1305715042882,30.2353661447208,30.3470744333655,30.4585844436019,
30.5699837411555,30.6813152383203,30.7926217504515,30.9040287727149,31.0154819353028,
31.1271517324974,31.2319470184472,31.3436553843173,31.4551654707913,31.5665648439344,
31.6778964159218,31.7892030019896,31.9006100962241,32.012063329828,32.123733195506,
32.2285278921736,32.3402364003461,32.4517466310075,32.5631461493833,32.6744778673927,
32.785784600018,32.8971918404589,33.0086452203188,33.1203152304052,33.2251087659,
33.3368166944272,33.4483263452669,33.5597252840978,33.6710564238063,33.7823625803406,
33.893769252746,34.0052220680331,34.1168915267853,34.2216896396264,34.3523579101859,
34.481718471605,34.5575191891205),.UNSPECIFIED.);
#845=B_SPLINE_CURVE_WITH_KNOTS('',3,(#8857,#8858,#8859,#8860,#8861,#8862,
#8863,#8864,#8865,#8866,#8867,#8868,#8869,#8870,#8871,#8872,#8873,#8874,
#8875,#8876,#8877,#8878,#8879,#8880,#8881,#8882,#8883,#8884,#8885,#8886,
#8887,#8888,#8889,#8890,#8891,#8892,#8893,#8894,#8895,#8896,#8897,#8898,
#8899,#8900,#8901,#8902,#8903,#8904,#8905,#8906,#8907,#8908,#8909,#8910,
#8911,#8912,#8913,#8914,#8915,#8916,#8917,#8918,#8919,#8920,#8921,#8922,
#8923,#8924,#8925,#8926,#8927,#8928,#8929,#8930,#8931,#8932,#8933,#8934,
#8935,#8936,#8937,#8938,#8939,#8940,#8941,#8942,#8943,#8944,#8945,#8946,
#8947,#8948,#8949,#8950,#8951,#8952,#8953,#8954,#8955,#8956,#8957,#8958,
#8959,#8960,#8961,#8962,#8963,#8964,#8965,#8966,#8967,#8968,#8969,#8970,
#8971,#8972,#8973,#8974,#8975,#8976,#8977,#8978,#8979,#8980,#8981,#8982,
#8983,#8984,#8985,#8986,#8987,#8988,#8989,#8990,#8991,#8992,#8993,#8994,
#8995,#8996),.UNSPECIFIED.,.F.,.F.,(4,2,2,2,2,2,2,2,2,2,2,2,2,2,2,2,2,2,
2,2,2,2,2,2,2,2,2,2,2,2,2,2,2,2,2,2,2,2,2,2,2,2,2,2,2,2,2,2,2,2,2,2,2,2,
2,2,2,2,2,2,2,2,2,2,2,2,2,2,2,4),(-0.980953657893252,-0.980813396397935,
-0.955825212739871,-0.943612668389274,-0.938075535682952,-0.933530523620638,
-0.926387108249715,-0.917187136880064,-0.891575066392669,-0.871442485613437,
-0.862182467834695,-0.854390254493591,-0.84427514937946,-0.82195729914483,
-0.790548017891759,-0.783957446457071,-0.779465309749546,-0.773592415631755,
-0.75534666273614,-0.717271876975574,-0.707538037175336,-0.699760128965384,
-0.690188684683091,-0.679464964866124,-0.657945149813074,-0.635181541542285,
-0.628511621408875,-0.624014213815331,-0.618198689398315,-0.600853494376346,
-0.567993231076083,-0.55548889750843,-0.547418543701117,-0.539090498054099,
-0.524821319297738,-0.504659878418917,-0.479565266719354,-0.472947877141004,
-0.468454504327042,-0.462602573191408,-0.444692631037342,-0.404807213794938,
-0.395563469735401,-0.387771635305561,-0.377638263679984,-0.355330862736666,
-0.32399450758584,-0.317395394883157,-0.312903502814609,-0.307038978128349,
-0.288918093124817,-0.249325569582235,-0.240067474399635,-0.232277288530633,
-0.222165390712545,-0.199853076120437,-0.168449642021253,-0.161861071291552,
-0.157370110224777,-0.151498510169382,-0.133253786386207,-0.0951955524731001,
-0.0854632416836036,-0.0776873239873771,-0.0681192646751081,-0.0392851986217844,
-0.0134167361551964,-0.00672038349945225,-0.0032887601749484,-0.000457478374081271),
 .UNSPECIFIED.);
#846=B_SPLINE_CURVE_WITH_KNOTS('',3,(#9001,#9002,#9003,#9004,#9005,#9006,
#9007,#9008,#9009,#9010,#9011,#9012,#9013,#9014,#9015,#9016,#9017,#9018,
#9019,#9020,#9021,#9022,#9023,#9024,#9025,#9026,#9027,#9028,#9029,#9030,
#9031,#9032,#9033,#9034,#9035,#9036,#9037,#9038,#9039,#9040,#9041,#9042,
#9043,#9044,#9045,#9046,#9047,#9048,#9049,#9050,#9051,#9052,#9053,#9054,
#9055,#9056,#9057,#9058,#9059,#9060,#9061,#9062,#9063,#9064,#9065,#9066,
#9067,#9068,#9069,#9070,#9071,#9072,#9073,#9074,#9075,#9076,#9077,#9078,
#9079,#9080,#9081,#9082,#9083,#9084,#9085,#9086,#9087,#9088,#9089,#9090,
#9091,#9092,#9093,#9094,#9095,#9096,#9097,#9098,#9099,#9100,#9101,#9102,
#9103,#9104,#9105,#9106,#9107,#9108,#9109,#9110,#9111,#9112,#9113,#9114,
#9115,#9116,#9117,#9118,#9119,#9120,#9121,#9122,#9123,#9124,#9125,#9126,
#9127,#9128,#9129,#9130,#9131,#9132,#9133,#9134,#9135,#9136,#9137,#9138,
#9139,#9140,#9141,#9142,#9143,#9144,#9145,#9146,#9147,#9148,#9149,#9150,
#9151,#9152,#9153,#9154,#9155,#9156,#9157,#9158,#9159,#9160,#9161,#9162,
#9163,#9164,#9165,#9166,#9167,#9168,#9169,#9170,#9171,#9172),
 .UNSPECIFIED.,.F.,.F.,(4,3,3,3,3,3,3,3,3,3,3,3,3,3,3,3,3,3,3,3,3,3,3,3,
3,3,3,3,3,3,3,3,3,3,3,3,3,3,3,3,3,3,3,3,3,3,3,3,3,3,3,3,3,3,3,3,3,4),(34.5575191894877,
34.6688302723381,34.7801258851517,34.8915360000216,35.0030001705123,35.1146924423315,
35.2182705133528,35.329979844159,35.4414909051851,35.5528912580536,35.6642238132373,
35.7755313842774,35.8869394583062,35.9983936704943,36.1100644998149,36.2148513870793,
36.3265566868323,36.4380637110229,36.5494600262282,36.6607885496869,36.7720921017016,
36.8834962086944,36.9949464756927,37.1066134484121,37.2114322608057,37.3231433221254,
37.4346560660442,37.5460580718723,37.6573922476748,37.76870140455,37.8801109978221,
37.9915666953808,38.1032389338652,38.2080131345321,38.3197270786042,38.4312428141906,
38.5426478756073,38.6539851650298,38.765297487747,38.8767103021909,38.9881692564661,
39.0998447680595,39.2045940082585,39.3162806032607,39.4277689172748,39.5391465312969,
39.6504563936481,39.7617413557063,39.8731271322649,39.9845591801971,40.0962083605028,
40.2011748819849,40.3134130635302,40.4254718990606,40.5373841223235,40.6492090027682,
40.7610153241071,40.8407044966673),.UNSPECIFIED.);
#847=B_SPLINE_CURVE_WITH_KNOTS('',3,(#9173,#9174,#9175,#9176,#9177,#9178,
#9179,#9180,#9181,#9182,#9183,#9184,#9185,#9186,#9187,#9188,#9189,#9190,
#9191,#9192,#9193,#9194,#9195,#9196,#9197,#9198,#9199,#9200,#9201,#9202,
#9203,#9204,#9205,#9206,#9207,#9208,#9209,#9210,#9211,#9212,#9213,#9214,
#9215,#9216,#9217,#9218,#9219,#9220,#9221,#9222,#9223,#9224,#9225,#9226,
#9227,#9228,#9229,#9230,#9231,#9232,#9233,#9234,#9235,#9236,#9237,#9238,
#9239,#9240,#9241,#9242,#9243,#9244,#9245,#9246,#9247,#9248,#9249,#9250,
#9251,#9252,#9253,#9254,#9255,#9256,#9257,#9258,#9259,#9260,#9261,#9262,
#9263,#9264,#9265,#9266,#9267,#9268,#9269,#9270,#9271,#9272,#9273,#9274,
#9275,#9276,#9277,#9278,#9279,#9280,#9281,#9282,#9283,#9284,#9285,#9286,
#9287,#9288,#9289,#9290,#9291,#9292,#9293,#9294,#9295,#9296,#9297,#9298,
#9299,#9300,#9301,#9302,#9303,#9304,#9305,#9306,#9307,#9308,#9309,#9310,
#9311,#9312,#9313,#9314,#9315,#9316,#9317,#9318,#9319,#9320,#9321,#9322,
#9323,#9324,#9325,#9326,#9327,#9328,#9329,#9330,#9331,#9332,#9333,#9334,
#9335,#9336,#9337,#9338,#9339,#9340,#9341,#9342,#9343,#9344),
 .UNSPECIFIED.,.F.,.F.,(4,3,3,3,3,3,3,3,3,3,3,3,3,3,3,3,3,3,3,3,3,3,3,3,
3,3,3,3,3,3,3,3,3,3,3,3,3,3,3,3,3,3,3,3,3,3,3,3,3,3,3,3,3,3,3,3,3,4),(34.557519189864,
34.6688316922454,34.7799480549331,34.8909555466978,35.0018977265956,35.1128180578458,
35.2238400790169,35.334912289609,35.4461940347629,35.5333624885445,35.6450709986202,
35.7565812311951,35.8679807514893,35.9793124714191,36.0906192059629,36.2020264483047,
36.3134798300591,36.4251498420039,36.5299433622709,36.6416512870095,36.7531609340692,
36.864559869128,36.9758910050783,37.0871971578746,37.1986038266028,37.3100566382399,
37.4217260934356,37.5265242359973,37.6382328481534,37.7497431759177,37.861142787168,
37.9724745937193,38.0837814104442,38.1951887274329,38.3066421798417,38.4183122548369,
38.5231051097237,38.634814450544,38.7463255216522,38.8577258846371,38.9690584499545,
39.0803660311285,39.1917741152101,39.3032283374232,39.4148991765908,39.5196859834501,
39.6313912609588,39.7428982629309,39.8542945559475,39.9656230572843,40.0769265872794,
40.1883306725875,40.2997809180481,40.4114478697587,40.5162668571765,40.6484523927198,
40.7791766765676,40.8407044966673),.UNSPECIFIED.);
#848=B_SPLINE_CURVE_WITH_KNOTS('',3,(#9349,#9350,#9351,#9352,#9353,#9354,
#9355,#9356,#9357,#9358,#9359,#9360,#9361,#9362,#9363,#9364,#9365,#9366,
#9367,#9368,#9369,#9370,#9371,#9372,#9373,#9374,#9375,#9376,#9377,#9378,
#9379,#9380,#9381,#9382,#9383,#9384,#9385,#9386,#9387,#9388,#9389,#9390,
#9391,#9392,#9393,#9394,#9395,#9396,#9397,#9398,#9399,#9400,#9401,#9402,
#9403,#9404,#9405,#9406,#9407,#9408,#9409,#9410,#9411,#9412,#9413,#9414,
#9415,#9416,#9417,#9418,#9419,#9420,#9421,#9422,#9423,#9424,#9425,#9426,
#9427,#9428,#9429,#9430,#9431,#9432,#9433,#9434,#9435,#9436,#9437,#9438,
#9439,#9440,#9441,#9442,#9443,#9444,#9445,#9446,#9447,#9448,#9449,#9450,
#9451,#9452,#9453,#9454,#9455,#9456,#9457,#9458,#9459,#9460,#9461,#9462,
#9463,#9464,#9465,#9466,#9467,#9468,#9469,#9470,#9471,#9472,#9473,#9474,
#9475,#9476,#9477,#9478,#9479,#9480,#9481,#9482,#9483,#9484,#9485,#9486,
#9487,#9488,#9489,#9490,#9491,#9492,#9493,#9494,#9495,#9496,#9497,#9498,
#9499,#9500,#9501,#9502,#9503,#9504,#9505,#9506,#9507,#9508,#9509,#9510,
#9511,#9512,#9513,#9514,#9515,#9516,#9517,#9518,#9519,#9520),
 .UNSPECIFIED.,.F.,.F.,(4,3,3,3,3,3,3,3,3,3,3,3,3,3,3,3,3,3,3,3,3,3,3,3,
3,3,3,3,3,3,3,3,3,3,3,3,3,3,3,3,3,3,3,3,3,3,3,3,3,3,3,3,3,3,3,3,3,4),(40.840704497049,
40.9675412582679,41.0954926672062,41.1977557557113,41.3094929575612,41.421032422769,
41.5324614834252,41.643822998072,41.755159728709,41.8665970369413,41.9780805721873,
42.0897804857431,42.1943366294377,42.3058933565765,42.4172516335834,42.5284991889107,
42.6396791835826,42.750834681469,42.8620926517494,42.9733975818198,43.0849224744629,
43.1909175031641,43.3028373726712,43.4145573215697,43.5261654134577,43.6377042144518,
43.7492161924285,43.8608241682442,43.972476138112,44.0843385386926,44.1874983768905,
44.2993486307196,44.4110045193044,44.5225519596468,44.6340335782541,44.7454919074656,
44.8570521214737,44.9686594749185,45.0804830762105,45.1840792506169,45.2946069224391,
45.4053635726771,45.5155858115154,45.6257438851437,45.7358823024636,45.8470767579335,
45.9573868777162,46.0690235010297,46.1806601243433,46.2985638342812,46.4122814276395,
46.5258600264502,46.6393375177506,46.7527516466314,46.8661750751564,46.9796037930555,
47.0931212124098,47.1238898038469),.UNSPECIFIED.);
#849=B_SPLINE_CURVE_WITH_KNOTS('',3,(#9521,#9522,#9523,#9524,#9525,#9526,
#9527,#9528,#9529,#9530),.UNSPECIFIED.,.F.,.F.,(4,1,1,1,1,1,1,4),(40.8407044966673,
41.5128477309029,42.5094286046293,43.5060094783558,44.5025903520822,45.4991712258086,
46.495752099535,47.1238898038469),.UNSPECIFIED.);
#850=B_SPLINE_CURVE_WITH_KNOTS('',3,(#9536,#9537,#9538,#9539,#9540,#9541,
#9542,#9543,#9544,#9545,#9546,#9547,#9548,#9549,#9550,#9551,#9552,#9553,
#9554,#9555,#9556,#9557,#9558,#9559,#9560,#9561,#9562,#9563,#9564,#9565,
#9566,#9567,#9568,#9569,#9570,#9571,#9572,#9573,#9574,#9575,#9576,#9577,
#9578,#9579,#9580,#9581,#9582,#9583,#9584,#9585,#9586,#9587,#9588,#9589,
#9590,#9591,#9592,#9593,#9594,#9595,#9596),.UNSPECIFIED.,.F.,.F.,(4,3,3,
3,3,3,3,3,3,3,3,3,3,3,3,3,3,3,3,3,4),(-4.0925417488383,-3.98632349490564,
-3.8806065760191,-3.77504892759528,-3.66961679425259,-3.56425173722768,
-3.45891795737562,-3.35357970118907,-3.24813369183657,-3.14262668426877,
-3.03694351958941,-2.98974262117923,-2.88522737486616,-2.78088717581065,
-2.67664451339593,-2.57246188586147,-2.4683018734843,-2.36405791614842,
-2.25977409419914,-2.15530886452125,-2.0655090872996),.UNSPECIFIED.);
#851=B_SPLINE_CURVE_WITH_KNOTS('',3,(#9599,#9600,#9601,#9602,#9603,#9604,
#9605,#9606,#9607,#9608,#9609,#9610,#9611,#9612,#9613,#9614,#9615,#9616,
#9617,#9618,#9619,#9620,#9621,#9622,#9623,#9624,#9625,#9626,#9627,#9628,
#9629,#9630,#9631,#9632),.UNSPECIFIED.,.F.,.F.,(4,3,3,3,3,3,3,3,3,3,3,4),
(0.,0.107961337641792,0.219038779652369,0.326921378979617,0.434806064728355,
0.542722047025971,0.656186753701081,0.764334836393998,0.872582285248723,
0.981026153163143,0.99658087372641,1.11419103802958),.UNSPECIFIED.);
#852=B_SPLINE_CURVE_WITH_KNOTS('',3,(#9637,#9638,#9639,#9640,#9641,#9642,
#9643,#9644,#9645,#9646,#9647,#9648,#9649,#9650,#9651,#9652,#9653,#9654,
#9655,#9656,#9657,#9658,#9659,#9660,#9661,#9662,#9663,#9664,#9665,#9666,
#9667,#9668,#9669,#9670,#9671,#9672,#9673,#9674,#9675,#9676,#9677,#9678,
#9679,#9680,#9681,#9682,#9683,#9684,#9685,#9686,#9687,#9688,#9689,#9690,
#9691,#9692,#9693,#9694,#9695,#9696,#9697,#9698,#9699,#9700,#9701,#9702,
#9703,#9704,#9705,#9706,#9707,#9708,#9709,#9710,#9711,#9712,#9713,#9714,
#9715,#9716,#9717,#9718,#9719,#9720,#9721,#9722,#9723,#9724,#9725,#9726,
#9727,#9728,#9729,#9730,#9731,#9732,#9733,#9734,#9735,#9736,#9737,#9738,
#9739,#9740,#9741,#9742,#9743,#9744,#9745,#9746,#9747,#9748,#9749,#9750,
#9751,#9752,#9753,#9754,#9755,#9756,#9757,#9758,#9759,#9760,#9761,#9762,
#9763,#9764,#9765,#9766,#9767,#9768,#9769,#9770,#9771,#9772,#9773,#9774,
#9775,#9776,#9777,#9778,#9779,#9780,#9781,#9782,#9783,#9784,#9785,#9786,
#9787,#9788,#9789,#9790,#9791,#9792,#9793,#9794,#9795,#9796,#9797,#9798,
#9799,#9800,#9801,#9802,#9803,#9804,#9805,#9806,#9807,#9808,#9809,#9810,
#9811,#9812,#9813,#9814,#9815,#9816,#9817,#9818,#9819,#9820,#9821,#9822,
#9823,#9824,#9825,#9826),.UNSPECIFIED.,.F.,.F.,(4,3,3,3,3,3,3,3,3,3,3,3,
3,3,3,3,3,3,3,3,3,3,3,3,3,3,3,3,3,3,3,3,3,3,3,3,3,3,3,3,3,3,3,3,3,3,3,3,
3,3,3,3,3,3,3,3,3,3,3,3,3,3,3,4),(-10.3757270556279,-10.2603201973078,-10.1445336437559,
-10.0282150027605,-9.96580873726409,-9.86028927215325,-9.75492847331709,
-9.64969134822421,-9.54452003581519,-9.43937844760692,-9.33423053922648,
-9.22897081685299,-9.12364803666882,-9.01814404094799,-8.96922786353768,
-8.86370563787302,-8.75834200872327,-8.65310196527416,-8.54792768174384,
-8.44278307461432,-8.33763210442475,-8.23236927738943,-8.12704336360686,
-8.02153622334535,-7.97264698981127,-7.86715075765798,-7.76181321062035,
-7.6565992534656,-7.55145104369272,-7.44633245870662,-7.34120741993228,
-7.23597021141746,-7.13066977480084,-7.02518762842015,-6.97606611608487,
-6.87052576919234,-6.76514418013918,-6.65988649813285,-6.55469478529848,
-6.44953298257136,-6.34436507518073,-6.23908581202828,-6.13374372441396,
-6.02822097903251,-5.97948524235845,-5.87394087033654,-5.76855477542758,
-5.66329190907334,-5.55809459516582,-5.45292678697872,-5.34775248164705,
-5.24246628022602,-5.137116936034,-5.03158652718211,-4.98290436863205,-4.87887809662516,
-4.77503069661956,-4.67128271432363,-4.56759611534961,-4.46393295588709,
-4.36019408038179,-4.25641481532146,-4.15247510001566,-4.09254174928664),
 .UNSPECIFIED.);
#853=B_SPLINE_CURVE_WITH_KNOTS('',3,(#9827,#9828,#9829,#9830,#9831,#9832,
#9833,#9834,#9835,#9836,#9837,#9838,#9839,#9840,#9841,#9842,#9843,#9844,
#9845,#9846,#9847,#9848,#9849,#9850,#9851,#9852,#9853,#9854,#9855,#9856,
#9857,#9858,#9859,#9860,#9861,#9862,#9863,#9864,#9865,#9866,#9867,#9868,
#9869,#9870,#9871,#9872,#9873,#9874,#9875,#9876,#9877,#9878,#9879,#9880,
#9881,#9882,#9883,#9884,#9885,#9886,#9887,#9888,#9889,#9890,#9891,#9892,
#9893,#9894,#9895,#9896,#9897,#9898,#9899,#9900,#9901,#9902,#9903,#9904,
#9905,#9906,#9907,#9908,#9909,#9910,#9911,#9912,#9913,#9914,#9915,#9916,
#9917,#9918,#9919,#9920,#9921,#9922,#9923,#9924,#9925,#9926,#9927,#9928,
#9929,#9930,#9931,#9932,#9933,#9934,#9935,#9936,#9937,#9938,#9939,#9940,
#9941,#9942,#9943,#9944,#9945,#9946,#9947,#9948,#9949,#9950,#9951,#9952,
#9953,#9954,#9955,#9956,#9957,#9958,#9959,#9960,#9961,#9962,#9963,#9964,
#9965,#9966,#9967,#9968,#9969,#9970,#9971,#9972,#9973,#9974,#9975,#9976,
#9977,#9978,#9979,#9980,#9981,#9982,#9983,#9984,#9985,#9986,#9987,#9988,
#9989,#9990,#9991,#9992,#9993,#9994,#9995,#9996,#9997,#9998,#9999,#10000,
#10001,#10002,#10003,#10004,#10005,#10006,#10007,#10008,#10009,#10010,#10011,
#10012,#10013,#10014,#10015,#10016),.UNSPECIFIED.,.F.,.F.,(4,3,3,3,3,3,
3,3,3,3,3,3,3,3,3,3,3,3,3,3,3,3,3,3,3,3,3,3,3,3,3,3,3,3,3,3,3,3,3,3,3,3,
3,3,3,3,3,3,3,3,3,3,3,3,3,3,3,3,3,3,3,3,3,4),(1.1141910384302,1.21724238536229,
1.32013451940758,1.42293952840389,1.52569615018617,1.62844303717372,1.73128762649966,
1.83418552892842,1.93726302853852,1.99316174745282,2.09882380530125,2.20432723759868,
2.30970630945701,2.41501904637471,2.52030130546123,2.6255888990106,2.73098582593673,
2.83644458423451,2.94208122698967,2.98974262117923,3.09543951511606,3.20098166055225,
3.30640502061617,3.41176548868121,3.51709885740447,3.62244087818947,3.72789690172061,
3.83341751346996,3.93911962813779,3.98632349490564,4.0917044614259,4.19692477051366,
4.30201914206295,4.40704637515871,4.51204277383473,4.61704459671652,4.72215786837924,
4.82733377201964,4.93269176979785,4.98290436863205,5.08844958739658,5.19383628319048,
5.29909938551099,5.40429670879907,5.50946430050027,5.61463816396031,5.71992358734267,
5.82527196030934,5.93080111180776,5.97948524235846,6.08502293419099,6.19040246033145,
6.29565896133579,6.40085004111363,6.50601175791134,6.61118012626058,6.71646067026086,
6.82180450898166,6.92732970844785,6.97606611608487,7.09145618049413,7.20651961582625,
7.32105406185355,7.39737634485402),.UNSPECIFIED.);
#854=B_SPLINE_CURVE_WITH_KNOTS('',3,(#10021,#10022,#10023,#10024,#10025,
#10026,#10027,#10028,#10029,#10030,#10031,#10032,#10033,#10034,#10035,#10036,
#10037,#10038,#10039,#10040,#10041,#10042,#10043,#10044,#10045,#10046,#10047,
#10048,#10049,#10050,#10051,#10052,#10053,#10054,#10055,#10056,#10057,#10058,
#10059,#10060,#10061,#10062,#10063,#10064,#10065,#10066,#10067,#10068,#10069,
#10070,#10071,#10072,#10073,#10074,#10075,#10076,#10077,#10078,#10079,#10080,
#10081,#10082,#10083,#10084,#10085,#10086,#10087,#10088,#10089,#10090,#10091,
#10092,#10093,#10094,#10095,#10096,#10097,#10098,#10099,#10100,#10101,#10102,
#10103,#10104,#10105,#10106,#10107,#10108,#10109,#10110,#10111,#10112,#10113,
#10114,#10115,#10116,#10117,#10118,#10119,#10120,#10121,#10122,#10123,#10124,
#10125,#10126,#10127,#10128,#10129,#10130,#10131,#10132,#10133,#10134,#10135,
#10136,#10137,#10138,#10139,#10140,#10141,#10142,#10143,#10144,#10145,#10146,
#10147,#10148,#10149,#10150,#10151,#10152,#10153,#10154,#10155,#10156,#10157,
#10158,#10159,#10160,#10161,#10162,#10163,#10164,#10165,#10166,#10167,#10168,
#10169,#10170,#10171,#10172,#10173,#10174,#10175,#10176,#10177,#10178,#10179,
#10180,#10181,#10182,#10183,#10184,#10185,#10186,#10187,#10188,#10189,#10190,
#10191,#10192,#10193,#10194,#10195,#10196,#10197,#10198,#10199,#10200,#10201,
#10202,#10203,#10204,#10205,#10206,#10207,#10208,#10209,#10210),
 .UNSPECIFIED.,.F.,.F.,(4,3,3,3,3,3,3,3,3,3,3,3,3,3,3,3,3,3,3,3,3,3,3,3,
3,3,3,3,3,3,3,3,3,3,3,3,3,3,3,3,3,3,3,3,3,3,3,3,3,3,3,3,3,3,3,3,3,3,3,3,
3,3,3,4),(-16.6589123631975,-16.5545511958811,-16.4502386019145,-16.3459373792312,
-16.2415362416226,-16.137085871038,-16.0324418402436,-15.9452939796226,
-15.8397770700368,-15.7344188085268,-15.6291841820779,-15.5240153429194,
-15.4188761990729,-15.3137307026416,-15.2084733274019,-15.1031528607631,
-14.9976511031837,-14.9487131058961,-14.8431960601418,-14.7378376610968,
-14.6326028957819,-14.5274339170148,-14.4222946330346,-14.3171489961608,
-14.2118914809822,-14.1065708744896,-14.0010689786592,-13.9521322321697,
-13.8466157393099,-13.7412578942317,-13.6360236817893,-13.5308552548952,
-13.4257165209662,-13.320571431498,-13.2153144560297,-13.1099943856376,
-13.0044930147749,-12.9555513584433,-12.8500342162662,-12.7446757247133,
-12.6394408730377,-12.5342718117636,-12.4291324492193,-12.323986737817,
-12.2187291546315,-12.1134084837545,-12.0079065297216,-11.9589704847169,
-11.8534526542618,-11.748093464529,-11.6428579035958,-11.5376881266243,
-11.4325480430808,-11.3274016065083,-11.2221432969162,-11.1168218978768,
-11.011319220686,-10.9623896109905,-10.8549891203279,-10.7477671220517,
-10.64071973154,-10.5337747634674,-10.4269036873047,-10.3757270560179),
 .UNSPECIFIED.);
#855=B_SPLINE_CURVE_WITH_KNOTS('',3,(#10211,#10212,#10213,#10214,#10215,
#10216,#10217,#10218,#10219,#10220,#10221,#10222,#10223,#10224,#10225,#10226,
#10227,#10228,#10229,#10230,#10231,#10232,#10233,#10234,#10235,#10236,#10237,
#10238,#10239,#10240,#10241,#10242,#10243,#10244,#10245,#10246,#10247,#10248,
#10249,#10250,#10251,#10252,#10253,#10254,#10255,#10256,#10257,#10258,#10259,
#10260,#10261,#10262,#10263,#10264,#10265,#10266,#10267,#10268,#10269,#10270,
#10271,#10272,#10273,#10274,#10275,#10276,#10277,#10278,#10279,#10280,#10281,
#10282,#10283,#10284,#10285,#10286,#10287,#10288,#10289,#10290,#10291,#10292,
#10293,#10294,#10295,#10296,#10297,#10298,#10299,#10300,#10301,#10302,#10303,
#10304,#10305,#10306,#10307,#10308,#10309,#10310,#10311,#10312,#10313,#10314,
#10315,#10316,#10317,#10318,#10319,#10320,#10321,#10322,#10323,#10324,#10325,
#10326,#10327,#10328,#10329,#10330,#10331,#10332,#10333,#10334,#10335,#10336,
#10337,#10338,#10339,#10340,#10341,#10342,#10343,#10344,#10345,#10346,#10347,
#10348,#10349,#10350,#10351,#10352,#10353,#10354,#10355,#10356,#10357,#10358,
#10359,#10360,#10361,#10362,#10363,#10364,#10365,#10366,#10367,#10368,#10369,
#10370,#10371,#10372,#10373,#10374,#10375,#10376,#10377,#10378,#10379,#10380,
#10381,#10382,#10383,#10384,#10385,#10386,#10387,#10388,#10389,#10390,#10391,
#10392,#10393,#10394,#10395,#10396,#10397,#10398,#10399,#10400),
 .UNSPECIFIED.,.F.,.F.,(4,3,3,3,3,3,3,3,3,3,3,3,3,3,3,3,3,3,3,3,3,3,3,3,
3,3,3,3,3,3,3,3,3,3,3,3,3,3,3,3,3,3,3,3,3,3,3,3,3,3,3,3,3,3,3,3,3,3,3,3,
3,3,3,4),(7.39737634520917,7.50456439630629,7.61181522811691,7.71924509232096,
7.82677710957531,7.93452849807945,7.97264698981128,8.07816920580473,8.18353281643424,
8.28877282842248,8.39394707248107,8.49909163221348,8.60424254715776,8.70950530751115,
8.81483114798237,8.92033820552726,8.96922786353769,9.07474698125424,9.18010750983923,
9.28534447958761,9.3905157080399,9.49565728357395,9.60080525053357,9.70606513833576,
9.81138814522112,9.91689245928984,9.96580873726409,10.0713229311903,10.1766784331036,
10.2819102485202,10.3870762463539,10.4922125229136,10.5973551303976,10.7026096036371,
10.8079271565927,10.913426012931,10.9623896109905,11.0679074212527,11.1732665931826,
11.278502139918,11.3836719049369,11.4888119787845,11.5939584079301,11.6992167135617,
11.8045381106151,11.9100407888698,11.9589704847169,12.0644875831434,12.1698460407086,
12.2750808729378,12.3802499237993,12.485389284951,12.590535003977,12.6957926083047,
12.8011133080766,12.9066153025981,12.9555513584433,13.0600577982311,13.1644187171345,
13.2686717663154,13.3728782799186,13.4770515526009,13.5812931985021,13.6805616523888),
 .UNSPECIFIED.);
#856=B_SPLINE_CURVE_WITH_KNOTS('',3,(#10405,#10406,#10407,#10408,#10409,
#10410,#10411,#10412,#10413,#10414,#10415),.UNSPECIFIED.,.F.,.F.,(4,1,1,
1,1,1,1,1,4),(-22.9420976703771,-22.9213600957074,-21.924779221981,-20.9281983482546,
-19.9316174745282,-18.9350366008018,-17.9384557270754,-16.941874853349,
-16.6589168227746),.UNSPECIFIED.);
#857=B_SPLINE_CURVE_WITH_KNOTS('',3,(#10416,#10417,#10418,#10419,#10420,
#10421,#10422,#10423,#10424,#10425,#10426,#10427,#10428,#10429,#10430,#10431,
#10432,#10433,#10434,#10435,#10436,#10437,#10438,#10439,#10440,#10441,#10442,
#10443,#10444,#10445,#10446,#10447,#10448,#10449,#10450,#10451,#10452,#10453,
#10454,#10455,#10456,#10457,#10458,#10459,#10460,#10461,#10462,#10463,#10464,
#10465,#10466,#10467,#10468,#10469,#10470,#10471,#10472,#10473,#10474,#10475,
#10476,#10477,#10478,#10479,#10480,#10481,#10482,#10483,#10484,#10485,#10486,
#10487,#10488,#10489,#10490,#10491,#10492,#10493,#10494,#10495,#10496,#10497,
#10498,#10499,#10500,#10501,#10502,#10503,#10504,#10505,#10506,#10507,#10508,
#10509,#10510,#10511,#10512,#10513,#10514,#10515,#10516,#10517,#10518,#10519,
#10520,#10521,#10522,#10523,#10524,#10525,#10526,#10527,#10528,#10529,#10530,
#10531,#10532,#10533,#10534,#10535,#10536,#10537,#10538,#10539,#10540,#10541,
#10542,#10543,#10544,#10545,#10546,#10547,#10548,#10549,#10550,#10551,#10552,
#10553,#10554,#10555,#10556,#10557,#10558,#10559,#10560,#10561,#10562,#10563,
#10564,#10565,#10566,#10567,#10568,#10569,#10570,#10571,#10572,#10573,#10574,
#10575,#10576,#10577,#10578,#10579,#10580,#10581,#10582,#10583,#10584,#10585,
#10586,#10587,#10588,#10589,#10590,#10591,#10592,#10593,#10594,#10595,#10596,
#10597,#10598,#10599,#10600,#10601,#10602,#10603,#10604,#10605),
 .UNSPECIFIED.,.F.,.F.,(4,3,3,3,3,3,3,3,3,3,3,3,3,3,3,3,3,3,3,3,3,3,3,3,
3,3,3,3,3,3,3,3,3,3,3,3,3,3,3,3,3,3,3,3,3,3,3,3,3,3,3,3,3,3,3,3,3,3,3,3,
3,3,3,4),(13.6805616528234,13.8163469424965,13.9521322321697,14.0576492724172,
14.1630076667916,14.2682424286898,14.3734114048201,14.4785506869449,14.5836963227474,
14.6889538380415,14.794274445328,14.8997763429847,14.9487131058961,15.0542300102651,
15.1595882677422,15.2648228919212,15.369991729905,15.4751308736699,15.5802763711125,
15.6855337490015,15.790854219229,15.8963559818009,15.9452939796226,16.0508108200795,
16.1561690120437,16.2614035686587,16.3665723378434,16.4717114116777,16.5768568381604,
16.6821141440126,16.7874345414828,16.8929362309438,16.941874853349,17.0473917665423,
17.1527500324105,17.2579846642936,17.3631535095492,17.4682926601413,17.5734381639534,
17.6786955474717,17.7840160229136,17.8895177900021,17.9384557270754,18.0439726204319,
18.1493308662541,18.2545654778812,18.3597343027628,18.4648734328942,18.5700189161903,
18.6752762792507,18.7805967342379,18.8860984810917,18.9350366008018,19.0405534775837,
19.1459117066389,19.251146301295,19.3563151090886,19.4614542220404,19.5665996880905,
19.6718570339202,19.7771774716605,19.8826792014212,19.9316174745282,19.9637469595683),
 .UNSPECIFIED.);
#858=B_SPLINE_CURVE_WITH_KNOTS('',3,(#10610,#10611,#10612,#10613,#10614,
#10615,#10616,#10617,#10618,#10619,#10620,#10621,#10622,#10623,#10624,#10625,
#10626,#10627,#10628,#10629,#10630,#10631,#10632,#10633,#10634,#10635,#10636,
#10637,#10638,#10639,#10640,#10641,#10642,#10643,#10644,#10645,#10646,#10647,
#10648,#10649,#10650,#10651,#10652,#10653,#10654,#10655,#10656,#10657,#10658,
#10659,#10660,#10661,#10662,#10663,#10664,#10665,#10666,#10667,#10668,#10669,
#10670,#10671,#10672,#10673,#10674,#10675,#10676,#10677,#10678,#10679,#10680,
#10681,#10682,#10683,#10684,#10685,#10686,#10687,#10688,#10689,#10690,#10691,
#10692,#10693,#10694,#10695,#10696,#10697,#10698,#10699,#10700,#10701,#10702,
#10703,#10704,#10705,#10706,#10707,#10708,#10709,#10710,#10711,#10712,#10713,
#10714,#10715,#10716,#10717,#10718,#10719,#10720,#10721,#10722,#10723,#10724,
#10725,#10726,#10727,#10728,#10729,#10730,#10731,#10732,#10733,#10734,#10735,
#10736,#10737,#10738,#10739,#10740,#10741,#10742,#10743,#10744,#10745,#10746,
#10747,#10748,#10749,#10750,#10751,#10752,#10753,#10754,#10755,#10756,#10757,
#10758,#10759,#10760,#10761,#10762,#10763,#10764,#10765,#10766,#10767,#10768,
#10769,#10770,#10771,#10772,#10773,#10774,#10775,#10776,#10777,#10778,#10779,
#10780,#10781,#10782,#10783,#10784,#10785,#10786,#10787,#10788,#10789,#10790,
#10791,#10792,#10793,#10794,#10795,#10796,#10797,#10798,#10799),
 .UNSPECIFIED.,.F.,.F.,(4,3,3,3,3,3,3,3,3,3,3,3,3,3,3,3,3,3,3,3,3,3,3,3,
3,3,3,3,3,3,3,3,3,3,3,3,3,3,3,3,3,3,3,3,3,3,3,3,3,3,3,3,3,3,3,3,3,3,3,3,
3,3,3,4),(-29.2252829771426,-29.1019668884045,-28.9772671757156,-28.9008453380659,
-28.7953311638248,-28.6899756819201,-28.584743886893,-28.4795779096737,
-28.3744416539223,-28.2692990674095,-28.1640446152455,-28.0587270834556,
-27.9532282482017,-27.9042644643395,-27.7987466448287,-27.6933874635457,
-27.5881519073483,-27.4829821328056,-27.3778420493868,-27.2726956106372,
-27.1674372954177,-27.0621158887715,-26.956613201017,-26.9076835906131,
-26.8021664914534,-26.696808033114,-26.5915732000532,-26.486404148325,-26.3812647862724,
-26.2761190663133,-26.1708614610085,-26.0655407602333,-25.9600387646782,
-25.9111027168866,-25.8055861967743,-25.7002283306547,-25.5949941064194,
-25.4898256734777,-25.3846869392368,-25.2795418551892,-25.1742848937338,
-25.0689648422825,-24.9634634977247,-24.9145218431602,-24.8090048011679,
-24.7036464050276,-24.5984116413407,-24.4932426634084,-24.3881033794713,
-24.2829577418491,-24.1777002247361,-24.0723796156286,-23.9668777161668,
-23.9179409694338,-23.8127945908852,-23.7039574758217,-23.5990948008806,
-23.494295154551,-23.3895219001086,-23.2847384419457,-23.1798422596674,
-23.0748784618845,-22.9697413145944,-22.9420976703771),.UNSPECIFIED.);
#859=B_SPLINE_CURVE_WITH_KNOTS('',3,(#10800,#10801,#10802,#10803,#10804,
#10805,#10806,#10807,#10808,#10809),.UNSPECIFIED.,.F.,.F.,(4,1,1,1,1,1,
1,4),(19.9637512898265,20.9281983482546,21.924779221981,22.9213600957074,
23.9179409694338,24.9145218431602,25.9111027168866,26.2469251046285),
 .UNSPECIFIED.);
#860=B_SPLINE_CURVE_WITH_KNOTS('',3,(#10814,#10815,#10816,#10817,#10818,
#10819,#10820,#10821,#10822,#10823,#10824,#10825,#10826,#10827,#10828,#10829,
#10830,#10831,#10832,#10833,#10834,#10835,#10836,#10837,#10838,#10839,#10840,
#10841,#10842,#10843,#10844,#10845,#10846,#10847,#10848,#10849,#10850,#10851,
#10852,#10853,#10854,#10855,#10856,#10857,#10858,#10859,#10860,#10861,#10862,
#10863,#10864,#10865,#10866,#10867,#10868,#10869,#10870,#10871,#10872,#10873,
#10874,#10875,#10876,#10877,#10878,#10879,#10880,#10881,#10882,#10883,#10884,
#10885,#10886,#10887,#10888,#10889,#10890,#10891,#10892,#10893,#10894,#10895,
#10896,#10897,#10898,#10899,#10900,#10901,#10902,#10903,#10904,#10905,#10906,
#10907,#10908,#10909,#10910,#10911,#10912,#10913,#10914,#10915,#10916,#10917,
#10918,#10919,#10920,#10921,#10922,#10923,#10924,#10925,#10926,#10927,#10928,
#10929,#10930,#10931,#10932,#10933,#10934,#10935,#10936,#10937,#10938,#10939,
#10940,#10941,#10942,#10943,#10944,#10945,#10946,#10947,#10948,#10949,#10950,
#10951,#10952,#10953,#10954,#10955,#10956,#10957,#10958,#10959,#10960,#10961,
#10962,#10963,#10964,#10965,#10966,#10967,#10968,#10969,#10970,#10971,#10972,
#10973,#10974,#10975,#10976,#10977,#10978,#10979,#10980,#10981,#10982,#10983,
#10984,#10985,#10986,#10987,#10988,#10989,#10990,#10991,#10992,#10993,#10994,
#10995,#10996,#10997,#10998,#10999,#11000,#11001,#11002,#11003),
 .UNSPECIFIED.,.F.,.F.,(4,3,3,3,3,3,3,3,3,3,3,3,3,3,3,3,3,3,3,3,3,3,3,3,
3,3,3,3,3,3,3,3,3,3,3,3,3,3,3,3,3,3,3,3,3,3,3,3,3,3,3,3,3,3,3,3,3,3,3,3,
3,3,3,4),(-35.5084682847362,-35.4023595064501,-35.2962353664596,-35.1899767723764,
-35.0836517048972,-34.9771072128199,-34.8803305804243,-34.7749501203421,
-34.6697303251661,-34.5646364761803,-34.4596097707505,-34.3546139040871,
-34.2496126168137,-34.1444998826443,-34.0393245183888,-33.9339670573156,
-33.8837497066979,-33.7782042662089,-33.6728173464077,-33.5675540178139,
-33.4623564669826,-33.3571886468187,-33.2520145543263,-33.1467289026185,
-33.0413803014021,-32.9358509241569,-32.8871688329715,-32.7816310902557,
-32.6762515117445,-32.5709949564141,-32.4658038211253,-32.3606420477126,
-32.2554736217241,-32.1501930189172,-32.0448491206365,-31.9393238610625,
-31.8905879592451,-31.7850905501633,-31.6797520943827,-31.5745376278472,
-31.4693891567628,-31.3642705581269,-31.2591457532205,-31.1539091496212,
-31.048609530701,-30.9431285201143,-30.8940070855187,-30.7884848231672,
-30.6831211656921,-30.5778811063684,-30.472706814698,-30.3675622071504,
-30.2624112442604,-30.1571484360913,-30.0518225478093,-29.9463154429612,
-29.8974262117923,-29.792124966494,-29.6869771514363,-29.58194618625,-29.4769877321303,
-29.3720711679708,-29.2671322858916,-29.2252829775567),.UNSPECIFIED.);
#861=B_SPLINE_CURVE_WITH_KNOTS('',3,(#11004,#11005,#11006,#11007,#11008,
#11009,#11010,#11011,#11012,#11013,#11014,#11015,#11016,#11017,#11018,#11019,
#11020,#11021,#11022,#11023,#11024,#11025,#11026,#11027,#11028,#11029,#11030,
#11031,#11032,#11033,#11034,#11035,#11036,#11037,#11038,#11039,#11040,#11041,
#11042,#11043,#11044,#11045,#11046,#11047,#11048,#11049,#11050,#11051,#11052,
#11053,#11054,#11055,#11056,#11057,#11058,#11059,#11060,#11061,#11062,#11063,
#11064,#11065,#11066,#11067,#11068,#11069,#11070,#11071,#11072,#11073,#11074,
#11075,#11076,#11077,#11078,#11079,#11080,#11081,#11082,#11083,#11084,#11085,
#11086,#11087,#11088,#11089,#11090,#11091,#11092,#11093,#11094,#11095,#11096,
#11097,#11098,#11099,#11100,#11101,#11102,#11103,#11104,#11105,#11106,#11107,
#11108,#11109,#11110,#11111,#11112,#11113,#11114,#11115,#11116,#11117,#11118,
#11119,#11120,#11121,#11122,#11123,#11124,#11125,#11126,#11127,#11128,#11129,
#11130,#11131,#11132,#11133,#11134,#11135,#11136,#11137,#11138,#11139,#11140,
#11141,#11142,#11143,#11144,#11145,#11146,#11147,#11148,#11149,#11150,#11151,
#11152,#11153,#11154,#11155,#11156,#11157,#11158,#11159,#11160,#11161,#11162,
#11163,#11164,#11165,#11166,#11167,#11168,#11169,#11170,#11171,#11172,#11173,
#11174,#11175,#11176,#11177,#11178,#11179,#11180,#11181,#11182,#11183,#11184,
#11185,#11186,#11187,#11188,#11189,#11190,#11191,#11192,#11193),
 .UNSPECIFIED.,.F.,.F.,(4,3,3,3,3,3,3,3,3,3,3,3,3,3,3,3,3,3,3,3,3,3,3,3,
3,3,3,3,3,3,3,3,3,3,3,3,3,3,3,3,3,3,3,3,3,3,3,3,3,3,3,3,3,3,3,3,3,3,3,3,
3,3,3,4),(26.2469322667479,26.3520739127528,26.4572007025229,26.5623485411171,
26.6676237508216,26.7729747238682,26.8785103872484,26.9076835906131,27.0132014116089,
27.118560591826,27.2237961432062,27.3289659106069,27.4341059845772,27.5392524115874,
27.6445107116996,27.7498321012928,27.8553347691868,27.9042644643395,28.0097784777039,
28.1151338402059,28.2203655774865,28.3255315352489,28.4306678097396,28.5358104531349,
28.6410650192122,28.7463826976556,28.8518817282743,28.9008453380659,29.0063647936612,
29.1117255831178,29.2169626990725,29.3221340024981,29.4272755818894,29.5324234816313,
29.6376831956907,29.7430059677339,29.8485099556615,29.8974262117923,30.0029483903628,
30.108311972099,30.2135519678941,30.3187262036494,30.4238707629554,30.5290216853458,
30.6342844649438,30.7396103314271,30.8451174250958,30.8940070855187,30.9995034308466,
31.1048410912431,31.2100551614913,31.3152034841296,31.4203221815889,31.5254473322794,
31.6306846511212,31.7359851973193,31.8414674509992,31.8905879592451,31.9966053193322,
32.1024616306615,32.209375616478,32.3150131087613,32.4225653413444,32.5301175739275),
 .UNSPECIFIED.);
#862=B_SPLINE_CURVE_WITH_KNOTS('',3,(#11196,#11197,#11198,#11199,#11200,
#11201,#11202,#11203,#11204,#11205,#11206,#11207,#11208,#11209,#11210,#11211,
#11212,#11213,#11214,#11215,#11216,#11217,#11218,#11219,#11220,#11221,#11222,
#11223,#11224,#11225,#11226,#11227,#11228,#11229,#11230,#11231,#11232,#11233,
#11234,#11235,#11236,#11237,#11238,#11239,#11240,#11241,#11242,#11243,#11244,
#11245,#11246,#11247,#11248,#11249,#11250,#11251,#11252,#11253,#11254,#11255,
#11256,#11257,#11258,#11259,#11260,#11261,#11262,#11263,#11264,#11265,#11266,
#11267,#11268,#11269,#11270,#11271,#11272,#11273,#11274,#11275,#11276,#11277,
#11278,#11279,#11280,#11281,#11282,#11283,#11284,#11285,#11286,#11287,#11288,
#11289,#11290,#11291,#11292,#11293,#11294,#11295,#11296,#11297,#11298,#11299,
#11300,#11301,#11302,#11303,#11304,#11305,#11306,#11307,#11308,#11309,#11310,
#11311,#11312,#11313,#11314,#11315,#11316,#11317,#11318,#11319,#11320,#11321,
#11322),.UNSPECIFIED.,.F.,.F.,(4,3,3,3,3,3,3,3,3,3,3,3,3,3,3,3,3,3,3,3,
3,3,3,3,3,3,3,3,3,3,3,3,3,3,3,3,3,3,3,3,3,3,4),(32.5301175743904,32.6499243852402,
32.7707627025493,32.8871688329715,32.9927129802535,33.0980988488266,33.2033614876022,
33.3085585732965,33.4137261529852,33.5189002298822,33.6241862045267,33.7295353225628,
33.835065508577,33.8837497066979,33.9891233821121,34.0943380597534,34.1994292723218,
34.3044548813995,34.4094511884809,34.5144544512916,34.6195714611784,34.7247524196896,
34.8301174455498,34.8803305804243,34.9860472709756,35.0916046934768,35.1970366054675,
35.3024014441108,35.4077350088512,35.5130730534988,35.6185188580415,35.724025664367,
35.8297086352625,35.8769114541507,35.9814256971422,36.085764885428,36.1900065327749,
36.2941881420584,36.3983471341029,36.502590073869,36.6068728780942,36.7113371001606,
36.8011443739907),.UNSPECIFIED.);
#863=B_SPLINE_CURVE_WITH_KNOTS('',3,(#11325,#11326,#11327,#11328,#11329,
#11330,#11331),.UNSPECIFIED.,.F.,.F.,(4,1,1,1,4),(-38.86665407533,-37.8700732016036,
-36.8734923278771,-35.8769114541507,-35.5084758780373),.UNSPECIFIED.);
#864=B_SPLINE_CURVE_WITH_KNOTS('',3,(#11334,#11335,#11336,#11337,#11338,
#11339,#11340,#11341,#11342,#11343,#11344,#11345,#11346,#11347,#11348,#11349,
#11350,#11351,#11352,#11353,#11354,#11355,#11356,#11357,#11358,#11359,#11360,
#11361,#11362,#11363,#11364,#11365,#11366,#11367,#11368,#11369,#11370),
 .UNSPECIFIED.,.F.,.F.,(4,3,3,3,3,3,3,3,3,3,3,3,4),(47.1238898038469,47.2495729833432,
47.3762357179408,47.4923329732614,47.6078590787388,47.7183089200037,47.8286551120703,
47.9389421371105,48.0492143835049,48.1595854549815,48.2700151013785,48.3806268044217,
48.4165418170808),.UNSPECIFIED.);
#865=B_SPLINE_CURVE_WITH_KNOTS('',3,(#11373,#11374,#11375,#11376,#11377,
#11378),.UNSPECIFIED.,.F.,.F.,(4,2,4),(9.70317678907225E-6,0.00416850045813341,
0.00832730327467254),.UNSPECIFIED.);
#866=B_SPLINE_CURVE_WITH_KNOTS('',3,(#11547,#11548,#11549,#11550,#11551,
#11552,#11553,#11554,#11555,#11556,#11557,#11558,#11559,#11560,#11561,#11562,
#11563,#11564,#11565,#11566,#11567,#11568,#11569,#11570,#11571,#11572,#11573,
#11574,#11575,#11576,#11577,#11578,#11579,#11580,#11581,#11582,#11583,#11584,
#11585,#11586,#11587,#11588,#11589,#11590,#11591,#11592,#11593,#11594,#11595,
#11596,#11597,#11598,#11599,#11600,#11601,#11602,#11603,#11604,#11605,#11606,
#11607,#11608,#11609,#11610,#11611,#11612,#11613,#11614,#11615,#11616,#11617,
#11618,#11619,#11620,#11621,#11622,#11623,#11624,#11625,#11626,#11627,#11628,
#11629,#11630,#11631,#11632,#11633,#11634),.UNSPECIFIED.,.F.,.F.,(4,3,3,
3,3,3,3,3,3,3,3,3,3,3,3,3,3,3,3,3,3,3,3,3,3,3,3,3,3,4),(0.,0.0141071418350746,
0.0355442789019995,0.0572656760904613,0.06697208668337,0.0731473068625853,
0.0768712321996411,0.0979621356483863,0.118760026435482,0.139128689171148,
0.144047130561891,0.148652874160775,0.168817015624542,0.188376963144646,
0.19974270647635,0.210158636009444,0.214504663212601,0.217541294027054,
0.237154834633298,0.25693437910066,0.270710750298301,0.279046676838732,
0.283673142787779,0.30272570932202,0.318739227454765,0.32422732905593,0.328196248012664,
0.346653672874964,0.365111097737263,0.366397579005847),.UNSPECIFIED.);
#867=B_SPLINE_CURVE_WITH_KNOTS('',3,(#11635,#11636,#11637,#11638,#11639,
#11640,#11641,#11642,#11643,#11644,#11645,#11646,#11647,#11648,#11649,#11650,
#11651,#11652,#11653,#11654,#11655,#11656,#11657,#11658,#11659,#11660,#11661,
#11662,#11663,#11664,#11665,#11666,#11667,#11668,#11669,#11670,#11671,#11672,
#11673,#11674,#11675,#11676,#11677,#11678,#11679,#11680,#11681,#11682,#11683,
#11684,#11685,#11686,#11687,#11688,#11689,#11690,#11691,#11692,#11693,#11694,
#11695,#11696,#11697,#11698,#11699,#11700,#11701,#11702,#11703,#11704,#11705,
#11706,#11707,#11708,#11709,#11710,#11711,#11712,#11713,#11714,#11715,#11716,
#11717,#11718,#11719,#11720,#11721,#11722),.UNSPECIFIED.,.F.,.F.,(4,3,3,
3,3,3,3,3,3,3,3,3,3,3,3,3,3,3,3,3,3,3,3,3,3,3,3,3,3,4),(0.,0.0113475426890351,
0.0291670472690302,0.0475729928382081,0.0560296921941146,0.0601609064744176,
0.0640260637775195,0.0829599659512082,0.102409502742518,0.121425659695721,
0.125492936123647,0.128447152834782,0.148489790009647,0.168489720572082,
0.178766369133891,0.190382802806189,0.193958991929988,0.213661586205272,
0.234044797116619,0.250281897850443,0.259921705842752,0.263839735831979,
0.267527540815499,0.288775631126542,0.307651155122482,0.313183531167478,
0.32004907337882,0.341698300745877,0.360810180211172,0.364629307890663),
 .UNSPECIFIED.);
#868=B_SPLINE_CURVE_WITH_KNOTS('',3,(#11891,#11892,#11893,#11894,#11895,
#11896,#11897,#11898,#11899,#11900,#11901,#11902,#11903,#11904,#11905,#11906,
#11907,#11908,#11909,#11910,#11911,#11912,#11913,#11914,#11915,#11916,#11917,
#11918,#11919,#11920,#11921,#11922,#11923,#11924,#11925,#11926,#11927,#11928,
#11929,#11930,#11931,#11932,#11933,#11934,#11935,#11936,#11937,#11938,#11939,
#11940,#11941,#11942,#11943,#11944,#11945,#11946,#11947,#11948,#11949,#11950,
#11951,#11952,#11953,#11954,#11955,#11956,#11957,#11958,#11959,#11960,#11961,
#11962,#11963,#11964,#11965,#11966,#11967,#11968,#11969,#11970,#11971,#11972,
#11973,#11974,#11975,#11976,#11977,#11978),.UNSPECIFIED.,.F.,.F.,(4,3,3,
3,3,3,3,3,3,3,3,3,3,3,3,3,3,3,3,3,3,3,3,3,3,3,3,3,3,4),(0.,0.0113475426890348,
0.0291670043807534,0.0475729266099651,0.0560296567510807,0.0601608189473537,
0.0640260370044265,0.0829599116369005,0.102409445900677,0.121425612301813,
0.125492777386276,0.128446963922241,0.148489595599423,0.168489527822768,
0.178766369133891,0.19038280280619,0.193958992762406,0.213737700534491,
0.233952427821611,0.254598689423448,0.25992170946175,0.263839753817461,
0.267527548191952,0.288775627561601,0.307651148863046,0.313183536175324,
0.317664301192065,0.339328429314369,0.360810221497805,0.364629307890676),
 .UNSPECIFIED.);
#869=B_SPLINE_CURVE_WITH_KNOTS('',3,(#11979,#11980,#11981,#11982,#11983,
#11984,#11985,#11986,#11987,#11988,#11989,#11990,#11991,#11992,#11993,#11994,
#11995,#11996,#11997,#11998,#11999,#12000,#12001,#12002,#12003,#12004,#12005,
#12006,#12007,#12008,#12009,#12010,#12011,#12012,#12013,#12014,#12015,#12016,
#12017,#12018,#12019,#12020,#12021,#12022,#12023,#12024,#12025,#12026,#12027,
#12028,#12029,#12030,#12031,#12032,#12033,#12034,#12035,#12036,#12037,#12038,
#12039,#12040,#12041,#12042,#12043,#12044,#12045,#12046,#12047,#12048,#12049,
#12050,#12051,#12052,#12053,#12054,#12055,#12056,#12057,#12058,#12059,#12060,
#12061,#12062,#12063,#12064,#12065,#12066),.UNSPECIFIED.,.F.,.F.,(4,3,3,
3,3,3,3,3,3,3,3,3,3,3,3,3,3,3,3,3,3,3,3,3,3,3,3,3,3,4),(0.,0.0141071418350769,
0.0355442756622905,0.0572656706841107,0.0669721763873351,0.0731472545815266,
0.0768712310065397,0.097962134032381,0.118760002271128,0.139128677510718,
0.144047115685023,0.148652871054896,0.168816990652203,0.188376892480646,
0.199742706476349,0.210158636009442,0.214504668206205,0.217541304167668,
0.237154819513473,0.256934375573258,0.270710752081222,0.2790466832613,0.284344214540952,
0.303389571149022,0.318739247434016,0.324227244433163,0.328196234496932,
0.346653692953416,0.3651111514099,0.366397579005838),.UNSPECIFIED.);
#870=VERTEX_POINT('',#3433);
#871=VERTEX_POINT('',#3434);
#872=VERTEX_POINT('',#3453);
#873=VERTEX_POINT('',#3486);
#874=VERTEX_POINT('',#3488);
#875=VERTEX_POINT('',#3526);
#876=VERTEX_POINT('',#3528);
#877=VERTEX_POINT('',#3530);
#878=VERTEX_POINT('',#3543);
#879=VERTEX_POINT('',#3556);
#880=VERTEX_POINT('',#3576);
#881=VERTEX_POINT('',#3578);
#882=VERTEX_POINT('',#3589);
#883=VERTEX_POINT('',#3619);
#884=VERTEX_POINT('',#3620);
#885=VERTEX_POINT('',#3622);
#886=VERTEX_POINT('',#3624);
#887=VERTEX_POINT('',#3628);
#888=VERTEX_POINT('',#3630);
#889=VERTEX_POINT('',#3634);
#890=VERTEX_POINT('',#3638);
#891=VERTEX_POINT('',#3642);
#892=VERTEX_POINT('',#3643);
#893=VERTEX_POINT('',#3645);
#894=VERTEX_POINT('',#3647);
#895=VERTEX_POINT('',#3651);
#896=VERTEX_POINT('',#3653);
#897=VERTEX_POINT('',#3657);
#898=VERTEX_POINT('',#3661);
#899=VERTEX_POINT('',#3665);
#900=VERTEX_POINT('',#3666);
#901=VERTEX_POINT('',#3668);
#902=VERTEX_POINT('',#3670);
#903=VERTEX_POINT('',#3674);
#904=VERTEX_POINT('',#3676);
#905=VERTEX_POINT('',#3680);
#906=VERTEX_POINT('',#3684);
#907=VERTEX_POINT('',#3688);
#908=VERTEX_POINT('',#3689);
#909=VERTEX_POINT('',#3691);
#910=VERTEX_POINT('',#3693);
#911=VERTEX_POINT('',#3697);
#912=VERTEX_POINT('',#3699);
#913=VERTEX_POINT('',#3703);
#914=VERTEX_POINT('',#3707);
#915=VERTEX_POINT('',#3711);
#916=VERTEX_POINT('',#3712);
#917=VERTEX_POINT('',#3714);
#918=VERTEX_POINT('',#3716);
#919=VERTEX_POINT('',#3720);
#920=VERTEX_POINT('',#3722);
#921=VERTEX_POINT('',#3726);
#922=VERTEX_POINT('',#3730);
#923=VERTEX_POINT('',#3734);
#924=VERTEX_POINT('',#3735);
#925=VERTEX_POINT('',#3737);
#926=VERTEX_POINT('',#3739);
#927=VERTEX_POINT('',#3743);
#928=VERTEX_POINT('',#3745);
#929=VERTEX_POINT('',#3749);
#930=VERTEX_POINT('',#3753);
#931=VERTEX_POINT('',#3757);
#932=VERTEX_POINT('',#3758);
#933=VERTEX_POINT('',#3760);
#934=VERTEX_POINT('',#3762);
#935=VERTEX_POINT('',#3766);
#936=VERTEX_POINT('',#3768);
#937=VERTEX_POINT('',#3772);
#938=VERTEX_POINT('',#3776);
#939=VERTEX_POINT('',#3780);
#940=VERTEX_POINT('',#3781);
#941=VERTEX_POINT('',#3783);
#942=VERTEX_POINT('',#3785);
#943=VERTEX_POINT('',#3789);
#944=VERTEX_POINT('',#3791);
#945=VERTEX_POINT('',#3795);
#946=VERTEX_POINT('',#3799);
#947=VERTEX_POINT('',#3803);
#948=VERTEX_POINT('',#3804);
#949=VERTEX_POINT('',#3806);
#950=VERTEX_POINT('',#3808);
#951=VERTEX_POINT('',#3812);
#952=VERTEX_POINT('',#3814);
#953=VERTEX_POINT('',#3818);
#954=VERTEX_POINT('',#3822);
#955=VERTEX_POINT('',#3826);
#956=VERTEX_POINT('',#3827);
#957=VERTEX_POINT('',#3829);
#958=VERTEX_POINT('',#3831);
#959=VERTEX_POINT('',#3835);
#960=VERTEX_POINT('',#3837);
#961=VERTEX_POINT('',#3841);
#962=VERTEX_POINT('',#3845);
#963=VERTEX_POINT('',#3849);
#964=VERTEX_POINT('',#3850);
#965=VERTEX_POINT('',#3852);
#966=VERTEX_POINT('',#3854);
#967=VERTEX_POINT('',#3858);
#968=VERTEX_POINT('',#3860);
#969=VERTEX_POINT('',#3864);
#970=VERTEX_POINT('',#3868);
#971=VERTEX_POINT('',#3872);
#972=VERTEX_POINT('',#3873);
#973=VERTEX_POINT('',#3875);
#974=VERTEX_POINT('',#3877);
#975=VERTEX_POINT('',#3881);
#976=VERTEX_POINT('',#3883);
#977=VERTEX_POINT('',#3887);
#978=VERTEX_POINT('',#3891);
#979=VERTEX_POINT('',#3895);
#980=VERTEX_POINT('',#3896);
#981=VERTEX_POINT('',#3898);
#982=VERTEX_POINT('',#3900);
#983=VERTEX_POINT('',#3904);
#984=VERTEX_POINT('',#3906);
#985=VERTEX_POINT('',#3910);
#986=VERTEX_POINT('',#3914);
#987=VERTEX_POINT('',#3918);
#988=VERTEX_POINT('',#3919);
#989=VERTEX_POINT('',#3921);
#990=VERTEX_POINT('',#3923);
#991=VERTEX_POINT('',#3927);
#992=VERTEX_POINT('',#3929);
#993=VERTEX_POINT('',#3933);
#994=VERTEX_POINT('',#3937);
#995=VERTEX_POINT('',#3941);
#996=VERTEX_POINT('',#3942);
#997=VERTEX_POINT('',#3944);
#998=VERTEX_POINT('',#3947);
#999=VERTEX_POINT('',#3949);
#1000=VERTEX_POINT('',#3965);
#1001=VERTEX_POINT('',#3969);
#1002=VERTEX_POINT('',#3971);
#1003=VERTEX_POINT('',#3975);
#1004=VERTEX_POINT('',#3979);
#1005=VERTEX_POINT('',#3985);
#1006=VERTEX_POINT('',#3988);
#1007=VERTEX_POINT('',#3991);
#1008=VERTEX_POINT('',#3995);
#1009=VERTEX_POINT('',#4000);
#1010=VERTEX_POINT('',#4004);
#1011=VERTEX_POINT('',#4007);
#1012=VERTEX_POINT('',#4011);
#1013=VERTEX_POINT('',#4015);
#1014=VERTEX_POINT('',#4020);
#1015=VERTEX_POINT('',#4024);
#1016=VERTEX_POINT('',#4027);
#1017=VERTEX_POINT('',#4031);
#1018=VERTEX_POINT('',#4035);
#1019=VERTEX_POINT('',#4038);
#1020=VERTEX_POINT('',#4042);
#1021=VERTEX_POINT('',#4049);
#1022=VERTEX_POINT('',#4050);
#1023=VERTEX_POINT('',#4052);
#1024=VERTEX_POINT('',#4201);
#1025=VERTEX_POINT('',#4316);
#1026=VERTEX_POINT('',#4317);
#1027=VERTEX_POINT('',#4340);
#1028=VERTEX_POINT('',#4341);
#1029=VERTEX_POINT('',#4652);
#1030=VERTEX_POINT('',#4653);
#1031=VERTEX_POINT('',#4970);
#1032=VERTEX_POINT('',#4971);
#1033=VERTEX_POINT('',#5318);
#1034=VERTEX_POINT('',#5319);
#1035=VERTEX_POINT('',#5504);
#1036=VERTEX_POINT('',#5505);
#1037=VERTEX_POINT('',#5507);
#1038=VERTEX_POINT('',#5569);
#1039=VERTEX_POINT('',#5606);
#1040=VERTEX_POINT('',#5607);
#1041=VERTEX_POINT('',#5990);
#1042=VERTEX_POINT('',#5991);
#1043=VERTEX_POINT('',#6374);
#1044=VERTEX_POINT('',#6375);
#1045=VERTEX_POINT('',#6579);
#1046=VERTEX_POINT('',#6580);
#1047=VERTEX_POINT('',#6783);
#1048=VERTEX_POINT('',#6784);
#1049=VERTEX_POINT('',#7167);
#1050=VERTEX_POINT('',#7295);
#1051=VERTEX_POINT('',#7305);
#1052=VERTEX_POINT('',#7343);
#1053=VERTEX_POINT('',#8037);
#1054=VERTEX_POINT('',#8038);
#1055=VERTEX_POINT('',#8040);
#1056=VERTEX_POINT('',#8042);
#1057=VERTEX_POINT('',#8044);
#1058=VERTEX_POINT('',#8046);
#1059=VERTEX_POINT('',#8050);
#1060=VERTEX_POINT('',#8052);
#1061=VERTEX_POINT('',#8056);
#1062=VERTEX_POINT('',#8060);
#1063=VERTEX_POINT('',#8064);
#1064=VERTEX_POINT('',#8068);
#1065=VERTEX_POINT('',#8077);
#1066=VERTEX_POINT('',#8078);
#1067=VERTEX_POINT('',#8080);
#1068=VERTEX_POINT('',#8229);
#1069=VERTEX_POINT('',#8344);
#1070=VERTEX_POINT('',#8345);
#1071=VERTEX_POINT('',#8368);
#1072=VERTEX_POINT('',#8369);
#1073=VERTEX_POINT('',#8682);
#1074=VERTEX_POINT('',#8683);
#1075=VERTEX_POINT('',#8998);
#1076=VERTEX_POINT('',#8999);
#1077=VERTEX_POINT('',#9346);
#1078=VERTEX_POINT('',#9347);
#1079=VERTEX_POINT('',#9532);
#1080=VERTEX_POINT('',#9533);
#1081=VERTEX_POINT('',#9535);
#1082=VERTEX_POINT('',#9597);
#1083=VERTEX_POINT('',#9634);
#1084=VERTEX_POINT('',#9635);
#1085=VERTEX_POINT('',#10018);
#1086=VERTEX_POINT('',#10019);
#1087=VERTEX_POINT('',#10402);
#1088=VERTEX_POINT('',#10403);
#1089=VERTEX_POINT('',#10607);
#1090=VERTEX_POINT('',#10608);
#1091=VERTEX_POINT('',#10811);
#1092=VERTEX_POINT('',#10812);
#1093=VERTEX_POINT('',#11195);
#1094=VERTEX_POINT('',#11323);
#1095=VERTEX_POINT('',#11333);
#1096=VERTEX_POINT('',#11371);
#1097=VERTEX_POINT('',#12068);
#1098=VERTEX_POINT('',#12069);
#1099=VERTEX_POINT('',#12071);
#1100=VERTEX_POINT('',#12073);
#1101=VERTEX_POINT('',#12075);
#1102=VERTEX_POINT('',#12077);
#1103=VERTEX_POINT('',#12081);
#1104=VERTEX_POINT('',#12083);
#1105=VERTEX_POINT('',#12087);
#1106=VERTEX_POINT('',#12091);
#1107=VERTEX_POINT('',#12095);
#1108=VERTEX_POINT('',#12099);
#1109=EDGE_CURVE('',#870,#871,#794,.T.);
#1110=EDGE_CURVE('',#872,#870,#795,.T.);
#1111=EDGE_CURVE('',#871,#872,#796,.T.);
#1112=EDGE_CURVE('',#871,#873,#518,.T.);
#1113=EDGE_CURVE('',#874,#873,#797,.T.);
#1114=EDGE_CURVE('',#873,#874,#798,.T.);
#1115=EDGE_CURVE('',#875,#875,#97,.T.);
#1116=EDGE_CURVE('',#875,#876,#519,.T.);
#1117=EDGE_CURVE('',#876,#877,#799,.T.);
#1118=EDGE_CURVE('',#877,#878,#800,.T.);
#1119=EDGE_CURVE('',#878,#879,#520,.T.);
#1120=EDGE_CURVE('',#879,#879,#98,.T.);
#1121=EDGE_CURVE('',#878,#870,#801,.T.);
#1122=EDGE_CURVE('',#872,#876,#802,.T.);
#1123=EDGE_CURVE('',#877,#880,#521,.T.);
#1124=EDGE_CURVE('',#881,#880,#803,.T.);
#1125=EDGE_CURVE('',#882,#881,#804,.T.);
#1126=EDGE_CURVE('',#880,#882,#805,.T.);
#1127=EDGE_CURVE('',#883,#884,#522,.T.);
#1128=EDGE_CURVE('',#883,#885,#99,.T.);
#1129=EDGE_CURVE('',#885,#886,#523,.T.);
#1130=EDGE_CURVE('',#886,#884,#100,.T.);
#1131=EDGE_CURVE('',#884,#887,#101,.T.);
#1132=EDGE_CURVE('',#888,#886,#102,.T.);
#1133=EDGE_CURVE('',#887,#888,#103,.T.);
#1134=EDGE_CURVE('',#889,#885,#104,.T.);
#1135=EDGE_CURVE('',#889,#888,#524,.T.);
#1136=EDGE_CURVE('',#887,#890,#525,.T.);
#1137=EDGE_CURVE('',#889,#890,#105,.T.);
#1138=EDGE_CURVE('',#891,#892,#526,.T.);
#1139=EDGE_CURVE('',#891,#893,#106,.T.);
#1140=EDGE_CURVE('',#893,#894,#527,.T.);
#1141=EDGE_CURVE('',#894,#892,#107,.T.);
#1142=EDGE_CURVE('',#892,#895,#108,.T.);
#1143=EDGE_CURVE('',#896,#894,#109,.T.);
#1144=EDGE_CURVE('',#895,#896,#110,.T.);
#1145=EDGE_CURVE('',#897,#893,#111,.T.);
#1146=EDGE_CURVE('',#897,#896,#528,.T.);
#1147=EDGE_CURVE('',#895,#898,#529,.T.);
#1148=EDGE_CURVE('',#897,#898,#112,.T.);
#1149=EDGE_CURVE('',#899,#900,#530,.T.);
#1150=EDGE_CURVE('',#899,#901,#113,.T.);
#1151=EDGE_CURVE('',#901,#902,#531,.T.);
#1152=EDGE_CURVE('',#902,#900,#114,.T.);
#1153=EDGE_CURVE('',#900,#903,#115,.T.);
#1154=EDGE_CURVE('',#904,#902,#116,.T.);
#1155=EDGE_CURVE('',#903,#904,#117,.T.);
#1156=EDGE_CURVE('',#905,#901,#118,.T.);
#1157=EDGE_CURVE('',#905,#904,#532,.T.);
#1158=EDGE_CURVE('',#903,#906,#533,.T.);
#1159=EDGE_CURVE('',#905,#906,#119,.T.);
#1160=EDGE_CURVE('',#907,#908,#534,.T.);
#1161=EDGE_CURVE('',#907,#909,#120,.T.);
#1162=EDGE_CURVE('',#909,#910,#535,.T.);
#1163=EDGE_CURVE('',#910,#908,#121,.T.);
#1164=EDGE_CURVE('',#908,#911,#122,.T.);
#1165=EDGE_CURVE('',#912,#910,#123,.T.);
#1166=EDGE_CURVE('',#911,#912,#124,.T.);
#1167=EDGE_CURVE('',#913,#909,#125,.T.);
#1168=EDGE_CURVE('',#913,#912,#536,.T.);
#1169=EDGE_CURVE('',#911,#914,#537,.T.);
#1170=EDGE_CURVE('',#913,#914,#126,.T.);
#1171=EDGE_CURVE('',#915,#916,#538,.T.);
#1172=EDGE_CURVE('',#915,#917,#127,.T.);
#1173=EDGE_CURVE('',#917,#918,#539,.T.);
#1174=EDGE_CURVE('',#918,#916,#128,.T.);
#1175=EDGE_CURVE('',#916,#919,#129,.T.);
#1176=EDGE_CURVE('',#920,#918,#130,.T.);
#1177=EDGE_CURVE('',#919,#920,#131,.T.);
#1178=EDGE_CURVE('',#921,#917,#132,.T.);
#1179=EDGE_CURVE('',#921,#920,#540,.T.);
#1180=EDGE_CURVE('',#919,#922,#541,.T.);
#1181=EDGE_CURVE('',#921,#922,#133,.T.);
#1182=EDGE_CURVE('',#923,#924,#542,.T.);
#1183=EDGE_CURVE('',#923,#925,#134,.T.);
#1184=EDGE_CURVE('',#925,#926,#543,.T.);
#1185=EDGE_CURVE('',#926,#924,#135,.T.);
#1186=EDGE_CURVE('',#924,#927,#136,.T.);
#1187=EDGE_CURVE('',#928,#926,#137,.T.);
#1188=EDGE_CURVE('',#927,#928,#138,.T.);
#1189=EDGE_CURVE('',#929,#925,#139,.T.);
#1190=EDGE_CURVE('',#929,#928,#544,.T.);
#1191=EDGE_CURVE('',#927,#930,#545,.T.);
#1192=EDGE_CURVE('',#929,#930,#140,.T.);
#1193=EDGE_CURVE('',#931,#932,#546,.T.);
#1194=EDGE_CURVE('',#931,#933,#141,.T.);
#1195=EDGE_CURVE('',#933,#934,#547,.T.);
#1196=EDGE_CURVE('',#934,#932,#142,.T.);
#1197=EDGE_CURVE('',#932,#935,#143,.T.);
#1198=EDGE_CURVE('',#936,#934,#144,.T.);
#1199=EDGE_CURVE('',#935,#936,#145,.T.);
#1200=EDGE_CURVE('',#937,#933,#146,.T.);
#1201=EDGE_CURVE('',#937,#936,#548,.T.);
#1202=EDGE_CURVE('',#935,#938,#549,.T.);
#1203=EDGE_CURVE('',#937,#938,#147,.T.);
#1204=EDGE_CURVE('',#939,#940,#550,.T.);
#1205=EDGE_CURVE('',#939,#941,#148,.T.);
#1206=EDGE_CURVE('',#941,#942,#551,.T.);
#1207=EDGE_CURVE('',#942,#940,#149,.T.);
#1208=EDGE_CURVE('',#940,#943,#150,.T.);
#1209=EDGE_CURVE('',#944,#942,#151,.T.);
#1210=EDGE_CURVE('',#943,#944,#152,.T.);
#1211=EDGE_CURVE('',#945,#941,#153,.T.);
#1212=EDGE_CURVE('',#945,#944,#552,.T.);
#1213=EDGE_CURVE('',#943,#946,#553,.T.);
#1214=EDGE_CURVE('',#945,#946,#154,.T.);
#1215=EDGE_CURVE('',#947,#948,#554,.T.);
#1216=EDGE_CURVE('',#947,#949,#155,.T.);
#1217=EDGE_CURVE('',#949,#950,#555,.T.);
#1218=EDGE_CURVE('',#950,#948,#156,.T.);
#1219=EDGE_CURVE('',#948,#951,#157,.T.);
#1220=EDGE_CURVE('',#952,#950,#158,.T.);
#1221=EDGE_CURVE('',#951,#952,#159,.T.);
#1222=EDGE_CURVE('',#953,#949,#160,.T.);
#1223=EDGE_CURVE('',#953,#952,#556,.T.);
#1224=EDGE_CURVE('',#951,#954,#557,.T.);
#1225=EDGE_CURVE('',#953,#954,#161,.T.);
#1226=EDGE_CURVE('',#955,#956,#558,.T.);
#1227=EDGE_CURVE('',#955,#957,#162,.T.);
#1228=EDGE_CURVE('',#957,#958,#559,.T.);
#1229=EDGE_CURVE('',#958,#956,#163,.T.);
#1230=EDGE_CURVE('',#956,#959,#164,.T.);
#1231=EDGE_CURVE('',#960,#958,#165,.T.);
#1232=EDGE_CURVE('',#959,#960,#166,.T.);
#1233=EDGE_CURVE('',#961,#957,#167,.T.);
#1234=EDGE_CURVE('',#961,#960,#560,.T.);
#1235=EDGE_CURVE('',#959,#962,#561,.T.);
#1236=EDGE_CURVE('',#961,#962,#168,.T.);
#1237=EDGE_CURVE('',#963,#964,#562,.T.);
#1238=EDGE_CURVE('',#963,#965,#169,.T.);
#1239=EDGE_CURVE('',#965,#966,#563,.T.);
#1240=EDGE_CURVE('',#966,#964,#170,.T.);
#1241=EDGE_CURVE('',#964,#967,#171,.T.);
#1242=EDGE_CURVE('',#968,#966,#172,.T.);
#1243=EDGE_CURVE('',#967,#968,#173,.T.);
#1244=EDGE_CURVE('',#969,#965,#174,.T.);
#1245=EDGE_CURVE('',#969,#968,#564,.T.);
#1246=EDGE_CURVE('',#967,#970,#565,.T.);
#1247=EDGE_CURVE('',#969,#970,#175,.T.);
#1248=EDGE_CURVE('',#971,#972,#566,.T.);
#1249=EDGE_CURVE('',#971,#973,#176,.T.);
#1250=EDGE_CURVE('',#973,#974,#567,.T.);
#1251=EDGE_CURVE('',#974,#972,#177,.T.);
#1252=EDGE_CURVE('',#972,#975,#178,.T.);
#1253=EDGE_CURVE('',#976,#974,#179,.T.);
#1254=EDGE_CURVE('',#975,#976,#180,.T.);
#1255=EDGE_CURVE('',#977,#973,#181,.T.);
#1256=EDGE_CURVE('',#977,#976,#568,.T.);
#1257=EDGE_CURVE('',#975,#978,#569,.T.);
#1258=EDGE_CURVE('',#977,#978,#182,.T.);
#1259=EDGE_CURVE('',#979,#980,#570,.T.);
#1260=EDGE_CURVE('',#979,#981,#183,.T.);
#1261=EDGE_CURVE('',#981,#982,#571,.T.);
#1262=EDGE_CURVE('',#982,#980,#184,.T.);
#1263=EDGE_CURVE('',#980,#983,#185,.T.);
#1264=EDGE_CURVE('',#984,#982,#186,.T.);
#1265=EDGE_CURVE('',#983,#984,#187,.T.);
#1266=EDGE_CURVE('',#985,#981,#188,.T.);
#1267=EDGE_CURVE('',#985,#984,#572,.T.);
#1268=EDGE_CURVE('',#983,#986,#573,.T.);
#1269=EDGE_CURVE('',#985,#986,#189,.T.);
#1270=EDGE_CURVE('',#987,#988,#574,.T.);
#1271=EDGE_CURVE('',#987,#989,#190,.T.);
#1272=EDGE_CURVE('',#989,#990,#575,.T.);
#1273=EDGE_CURVE('',#990,#988,#191,.T.);
#1274=EDGE_CURVE('',#988,#991,#192,.T.);
#1275=EDGE_CURVE('',#992,#990,#193,.T.);
#1276=EDGE_CURVE('',#991,#992,#194,.T.);
#1277=EDGE_CURVE('',#993,#989,#195,.T.);
#1278=EDGE_CURVE('',#993,#992,#576,.T.);
#1279=EDGE_CURVE('',#991,#994,#577,.T.);
#1280=EDGE_CURVE('',#993,#994,#196,.T.);
#1281=EDGE_CURVE('',#995,#996,#197,.T.);
#1282=EDGE_CURVE('',#996,#997,#578,.T.);
#1283=EDGE_CURVE('',#997,#997,#198,.T.);
#1284=EDGE_CURVE('',#996,#998,#199,.T.);
#1285=EDGE_CURVE('',#998,#999,#579,.T.);
#1286=EDGE_CURVE('',#883,#999,#200,.T.);
#1287=EDGE_CURVE('',#891,#890,#201,.T.);
#1288=EDGE_CURVE('',#899,#898,#202,.T.);
#1289=EDGE_CURVE('',#907,#906,#203,.T.);
#1290=EDGE_CURVE('',#915,#914,#204,.T.);
#1291=EDGE_CURVE('',#923,#922,#205,.T.);
#1292=EDGE_CURVE('',#931,#930,#206,.T.);
#1293=EDGE_CURVE('',#939,#938,#207,.T.);
#1294=EDGE_CURVE('',#947,#946,#208,.T.);
#1295=EDGE_CURVE('',#955,#954,#209,.T.);
#1296=EDGE_CURVE('',#963,#962,#210,.T.);
#1297=EDGE_CURVE('',#971,#970,#211,.T.);
#1298=EDGE_CURVE('',#979,#978,#212,.T.);
#1299=EDGE_CURVE('',#987,#986,#213,.T.);
#1300=EDGE_CURVE('',#1000,#994,#214,.T.);
#1301=EDGE_CURVE('',#1000,#995,#580,.T.);
#1302=EDGE_CURVE('',#1000,#1001,#215,.T.);
#1303=EDGE_CURVE('',#1001,#1002,#581,.T.);
#1304=EDGE_CURVE('',#1002,#995,#216,.T.);
#1305=EDGE_CURVE('',#1003,#1002,#217,.T.);
#1306=EDGE_CURVE('',#998,#1003,#218,.T.);
#1307=EDGE_CURVE('',#1004,#1001,#219,.T.);
#1308=EDGE_CURVE('',#1004,#1003,#582,.T.);
#1309=EDGE_CURVE('',#1004,#999,#220,.T.);
#1310=EDGE_CURVE('',#1005,#1005,#221,.T.);
#1311=EDGE_CURVE('',#1006,#1006,#222,.T.);
#1312=EDGE_CURVE('',#1007,#1007,#223,.T.);
#1313=EDGE_CURVE('',#1007,#1006,#583,.T.);
#1314=EDGE_CURVE('',#1008,#1008,#224,.T.);
#1315=EDGE_CURVE('',#1008,#881,#584,.T.);
#1316=EDGE_CURVE('',#882,#1007,#585,.T.);
#1317=EDGE_CURVE('',#1008,#1009,#586,.T.);
#1318=EDGE_CURVE('',#1009,#1009,#225,.T.);
#1319=EDGE_CURVE('',#1010,#1010,#226,.T.);
#1320=EDGE_CURVE('',#1011,#1011,#227,.T.);
#1321=EDGE_CURVE('',#1011,#1010,#587,.T.);
#1322=EDGE_CURVE('',#1011,#1012,#588,.T.);
#1323=EDGE_CURVE('',#1012,#1012,#228,.T.);
#1324=EDGE_CURVE('',#1013,#1013,#229,.T.);
#1325=EDGE_CURVE('',#879,#1013,#589,.T.);
#1326=EDGE_CURVE('',#875,#1014,#590,.T.);
#1327=EDGE_CURVE('',#1014,#1014,#230,.T.);
#1328=EDGE_CURVE('',#1015,#1015,#231,.T.);
#1329=EDGE_CURVE('',#1016,#1016,#232,.T.);
#1330=EDGE_CURVE('',#1016,#1015,#591,.T.);
#1331=EDGE_CURVE('',#1016,#1017,#592,.T.);
#1332=EDGE_CURVE('',#1017,#1017,#233,.T.);
#1333=EDGE_CURVE('',#1018,#1018,#234,.T.);
#1334=EDGE_CURVE('',#1019,#1019,#235,.T.);
#1335=EDGE_CURVE('',#1019,#1018,#593,.T.);
#1336=EDGE_CURVE('',#1020,#1020,#236,.T.);
#1337=EDGE_CURVE('',#1020,#1019,#594,.T.);
#1338=EDGE_CURVE('',#1020,#1005,#595,.T.);
#1339=EDGE_CURVE('',#1021,#1022,#596,.T.);
#1340=EDGE_CURVE('',#1023,#1021,#806,.T.);
#1341=EDGE_CURVE('',#1024,#1023,#237,.T.);
#1342=EDGE_CURVE('',#1024,#1022,#807,.T.);
#1343=EDGE_CURVE('',#1025,#1026,#597,.T.);
#1344=EDGE_CURVE('',#1021,#1025,#808,.T.);
#1345=EDGE_CURVE('',#1022,#1026,#809,.T.);
#1346=EDGE_CURVE('',#1027,#1028,#598,.T.);
#1347=EDGE_CURVE('',#1025,#1027,#810,.T.);
#1348=EDGE_CURVE('',#1026,#1028,#811,.T.);
#1349=EDGE_CURVE('',#1029,#1030,#599,.T.);
#1350=EDGE_CURVE('',#1027,#1029,#812,.T.);
#1351=EDGE_CURVE('',#1028,#1030,#813,.T.);
#1352=EDGE_CURVE('',#1031,#1032,#600,.T.);
#1353=EDGE_CURVE('',#1029,#1031,#814,.T.);
#1354=EDGE_CURVE('',#1030,#1032,#815,.T.);
#1355=EDGE_CURVE('',#1033,#1034,#601,.T.);
#1356=EDGE_CURVE('',#1031,#1033,#816,.T.);
#1357=EDGE_CURVE('',#1032,#1034,#817,.T.);
#1358=EDGE_CURVE('',#1035,#1036,#602,.T.);
#1359=EDGE_CURVE('',#1035,#1037,#818,.T.);
#1360=EDGE_CURVE('',#1037,#1038,#238,.F.);
#1361=EDGE_CURVE('',#1038,#1036,#819,.T.);
#1362=EDGE_CURVE('',#1039,#1040,#603,.T.);
#1363=EDGE_CURVE('',#1039,#1035,#820,.T.);
#1364=EDGE_CURVE('',#1036,#1040,#821,.T.);
#1365=EDGE_CURVE('',#1041,#1042,#604,.T.);
#1366=EDGE_CURVE('',#1041,#1039,#822,.T.);
#1367=EDGE_CURVE('',#1040,#1042,#823,.T.);
#1368=EDGE_CURVE('',#1043,#1044,#605,.T.);
#1369=EDGE_CURVE('',#1043,#1041,#824,.T.);
#1370=EDGE_CURVE('',#1042,#1044,#825,.T.);
#1371=EDGE_CURVE('',#1045,#1046,#606,.T.);
#1372=EDGE_CURVE('',#1045,#1043,#826,.T.);
#1373=EDGE_CURVE('',#1044,#1046,#827,.T.);
#1374=EDGE_CURVE('',#1047,#1048,#607,.T.);
#1375=EDGE_CURVE('',#1047,#1045,#828,.T.);
#1376=EDGE_CURVE('',#1046,#1048,#829,.T.);
#1377=EDGE_CURVE('',#1048,#1049,#830,.T.);
#1378=EDGE_CURVE('',#1050,#1049,#239,.F.);
#1379=EDGE_CURVE('',#1050,#1047,#831,.T.);
#1380=EDGE_CURVE('',#1034,#1051,#832,.T.);
#1381=EDGE_CURVE('',#1052,#1051,#240,.T.);
#1382=EDGE_CURVE('',#1033,#1052,#833,.T.);
#1383=EDGE_CURVE('',#1049,#1052,#834,.T.);
#1384=EDGE_CURVE('',#1023,#1038,#835,.T.);
#1385=EDGE_CURVE('',#1051,#1050,#836,.T.);
#1386=EDGE_CURVE('',#1037,#1024,#837,.T.);
#1387=EDGE_CURVE('',#1053,#1054,#608,.T.);
#1388=EDGE_CURVE('',#1054,#1055,#609,.T.);
#1389=EDGE_CURVE('',#1055,#1056,#610,.T.);
#1390=EDGE_CURVE('',#1056,#1057,#611,.T.);
#1391=EDGE_CURVE('',#1057,#1058,#612,.T.);
#1392=EDGE_CURVE('',#1058,#1053,#613,.T.);
#1393=EDGE_CURVE('',#1053,#1059,#614,.T.);
#1394=EDGE_CURVE('',#1059,#1060,#615,.T.);
#1395=EDGE_CURVE('',#1054,#1060,#616,.T.);
#1396=EDGE_CURVE('',#1058,#1061,#617,.T.);
#1397=EDGE_CURVE('',#1061,#1059,#618,.T.);
#1398=EDGE_CURVE('',#1057,#1062,#619,.T.);
#1399=EDGE_CURVE('',#1062,#1061,#620,.T.);
#1400=EDGE_CURVE('',#1056,#1063,#621,.T.);
#1401=EDGE_CURVE('',#1063,#1062,#622,.T.);
#1402=EDGE_CURVE('',#1055,#1064,#623,.T.);
#1403=EDGE_CURVE('',#1064,#1063,#624,.T.);
#1404=EDGE_CURVE('',#1060,#1064,#625,.T.);
#1405=EDGE_CURVE('',#1065,#1066,#626,.T.);
#1406=EDGE_CURVE('',#1067,#1065,#838,.T.);
#1407=EDGE_CURVE('',#1068,#1067,#241,.T.);
#1408=EDGE_CURVE('',#1068,#1066,#839,.T.);
#1409=EDGE_CURVE('',#1069,#1070,#627,.T.);
#1410=EDGE_CURVE('',#1065,#1069,#840,.T.);
#1411=EDGE_CURVE('',#1066,#1070,#841,.T.);
#1412=EDGE_CURVE('',#1071,#1072,#628,.T.);
#1413=EDGE_CURVE('',#1069,#1071,#842,.T.);
#1414=EDGE_CURVE('',#1070,#1072,#843,.T.);
#1415=EDGE_CURVE('',#1073,#1074,#629,.T.);
#1416=EDGE_CURVE('',#1071,#1073,#844,.T.);
#1417=EDGE_CURVE('',#1072,#1074,#845,.T.);
#1418=EDGE_CURVE('',#1075,#1076,#630,.T.);
#1419=EDGE_CURVE('',#1073,#1075,#846,.T.);
#1420=EDGE_CURVE('',#1074,#1076,#847,.T.);
#1421=EDGE_CURVE('',#1077,#1078,#631,.T.);
#1422=EDGE_CURVE('',#1075,#1077,#848,.T.);
#1423=EDGE_CURVE('',#1076,#1078,#849,.T.);
#1424=EDGE_CURVE('',#1079,#1080,#632,.T.);
#1425=EDGE_CURVE('',#1079,#1081,#850,.T.);
#1426=EDGE_CURVE('',#1081,#1082,#242,.F.);
#1427=EDGE_CURVE('',#1082,#1080,#851,.T.);
#1428=EDGE_CURVE('',#1083,#1084,#633,.T.);
#1429=EDGE_CURVE('',#1083,#1079,#852,.T.);
#1430=EDGE_CURVE('',#1080,#1084,#853,.T.);
#1431=EDGE_CURVE('',#1085,#1086,#634,.T.);
#1432=EDGE_CURVE('',#1085,#1083,#854,.T.);
#1433=EDGE_CURVE('',#1084,#1086,#855,.T.);
#1434=EDGE_CURVE('',#1087,#1088,#635,.T.);
#1435=EDGE_CURVE('',#1087,#1085,#856,.T.);
#1436=EDGE_CURVE('',#1086,#1088,#857,.T.);
#1437=EDGE_CURVE('',#1089,#1090,#636,.T.);
#1438=EDGE_CURVE('',#1089,#1087,#858,.T.);
#1439=EDGE_CURVE('',#1088,#1090,#859,.T.);
#1440=EDGE_CURVE('',#1091,#1092,#637,.T.);
#1441=EDGE_CURVE('',#1091,#1089,#860,.T.);
#1442=EDGE_CURVE('',#1090,#1092,#861,.T.);
#1443=EDGE_CURVE('',#1092,#1093,#862,.T.);
#1444=EDGE_CURVE('',#1094,#1093,#243,.F.);
#1445=EDGE_CURVE('',#1094,#1091,#863,.T.);
#1446=EDGE_CURVE('',#1078,#1095,#864,.T.);
#1447=EDGE_CURVE('',#1096,#1095,#244,.T.);
#1448=EDGE_CURVE('',#1077,#1096,#865,.T.);
#1449=EDGE_CURVE('',#1093,#1096,#866,.T.);
#1450=EDGE_CURVE('',#1067,#1082,#867,.T.);
#1451=EDGE_CURVE('',#1095,#1094,#868,.T.);
#1452=EDGE_CURVE('',#1081,#1068,#869,.T.);
#1453=EDGE_CURVE('',#1097,#1098,#638,.T.);
#1454=EDGE_CURVE('',#1098,#1099,#639,.T.);
#1455=EDGE_CURVE('',#1099,#1100,#640,.T.);
#1456=EDGE_CURVE('',#1100,#1101,#641,.T.);
#1457=EDGE_CURVE('',#1101,#1102,#642,.T.);
#1458=EDGE_CURVE('',#1102,#1097,#643,.T.);
#1459=EDGE_CURVE('',#1097,#1103,#644,.T.);
#1460=EDGE_CURVE('',#1103,#1104,#645,.T.);
#1461=EDGE_CURVE('',#1098,#1104,#646,.T.);
#1462=EDGE_CURVE('',#1102,#1105,#647,.T.);
#1463=EDGE_CURVE('',#1105,#1103,#648,.T.);
#1464=EDGE_CURVE('',#1101,#1106,#649,.T.);
#1465=EDGE_CURVE('',#1106,#1105,#650,.T.);
#1466=EDGE_CURVE('',#1100,#1107,#651,.T.);
#1467=EDGE_CURVE('',#1107,#1106,#652,.T.);
#1468=EDGE_CURVE('',#1099,#1108,#653,.T.);
#1469=EDGE_CURVE('',#1108,#1107,#654,.T.);
#1470=EDGE_CURVE('',#1104,#1108,#655,.T.);
#1471=ORIENTED_EDGE('',*,*,#1109,.F.);
#1472=ORIENTED_EDGE('',*,*,#1110,.F.);
#1473=ORIENTED_EDGE('',*,*,#1111,.F.);
#1474=ORIENTED_EDGE('',*,*,#1112,.T.);
#1475=ORIENTED_EDGE('',*,*,#1113,.F.);
#1476=ORIENTED_EDGE('',*,*,#1114,.F.);
#1477=ORIENTED_EDGE('',*,*,#1112,.F.);
#1478=ORIENTED_EDGE('',*,*,#1115,.F.);
#1479=ORIENTED_EDGE('',*,*,#1116,.T.);
#1480=ORIENTED_EDGE('',*,*,#1117,.T.);
#1481=ORIENTED_EDGE('',*,*,#1118,.T.);
#1482=ORIENTED_EDGE('',*,*,#1119,.T.);
#1483=ORIENTED_EDGE('',*,*,#1120,.T.);
#1484=ORIENTED_EDGE('',*,*,#1119,.F.);
#1485=ORIENTED_EDGE('',*,*,#1121,.T.);
#1486=ORIENTED_EDGE('',*,*,#1109,.T.);
#1487=ORIENTED_EDGE('',*,*,#1111,.T.);
#1488=ORIENTED_EDGE('',*,*,#1122,.T.);
#1489=ORIENTED_EDGE('',*,*,#1116,.F.);
#1490=ORIENTED_EDGE('',*,*,#1122,.F.);
#1491=ORIENTED_EDGE('',*,*,#1110,.T.);
#1492=ORIENTED_EDGE('',*,*,#1121,.F.);
#1493=ORIENTED_EDGE('',*,*,#1118,.F.);
#1494=ORIENTED_EDGE('',*,*,#1123,.T.);
#1495=ORIENTED_EDGE('',*,*,#1124,.F.);
#1496=ORIENTED_EDGE('',*,*,#1125,.F.);
#1497=ORIENTED_EDGE('',*,*,#1126,.F.);
#1498=ORIENTED_EDGE('',*,*,#1123,.F.);
#1499=ORIENTED_EDGE('',*,*,#1117,.F.);
#1500=ORIENTED_EDGE('',*,*,#1127,.F.);
#1501=ORIENTED_EDGE('',*,*,#1128,.T.);
#1502=ORIENTED_EDGE('',*,*,#1129,.T.);
#1503=ORIENTED_EDGE('',*,*,#1130,.T.);
#1504=ORIENTED_EDGE('',*,*,#1131,.F.);
#1505=ORIENTED_EDGE('',*,*,#1130,.F.);
#1506=ORIENTED_EDGE('',*,*,#1132,.F.);
#1507=ORIENTED_EDGE('',*,*,#1133,.F.);
#1508=ORIENTED_EDGE('',*,*,#1134,.F.);
#1509=ORIENTED_EDGE('',*,*,#1135,.T.);
#1510=ORIENTED_EDGE('',*,*,#1132,.T.);
#1511=ORIENTED_EDGE('',*,*,#1129,.F.);
#1512=ORIENTED_EDGE('',*,*,#1136,.F.);
#1513=ORIENTED_EDGE('',*,*,#1133,.T.);
#1514=ORIENTED_EDGE('',*,*,#1135,.F.);
#1515=ORIENTED_EDGE('',*,*,#1137,.T.);
#1516=ORIENTED_EDGE('',*,*,#1138,.F.);
#1517=ORIENTED_EDGE('',*,*,#1139,.T.);
#1518=ORIENTED_EDGE('',*,*,#1140,.T.);
#1519=ORIENTED_EDGE('',*,*,#1141,.T.);
#1520=ORIENTED_EDGE('',*,*,#1142,.F.);
#1521=ORIENTED_EDGE('',*,*,#1141,.F.);
#1522=ORIENTED_EDGE('',*,*,#1143,.F.);
#1523=ORIENTED_EDGE('',*,*,#1144,.F.);
#1524=ORIENTED_EDGE('',*,*,#1145,.F.);
#1525=ORIENTED_EDGE('',*,*,#1146,.T.);
#1526=ORIENTED_EDGE('',*,*,#1143,.T.);
#1527=ORIENTED_EDGE('',*,*,#1140,.F.);
#1528=ORIENTED_EDGE('',*,*,#1147,.F.);
#1529=ORIENTED_EDGE('',*,*,#1144,.T.);
#1530=ORIENTED_EDGE('',*,*,#1146,.F.);
#1531=ORIENTED_EDGE('',*,*,#1148,.T.);
#1532=ORIENTED_EDGE('',*,*,#1149,.F.);
#1533=ORIENTED_EDGE('',*,*,#1150,.T.);
#1534=ORIENTED_EDGE('',*,*,#1151,.T.);
#1535=ORIENTED_EDGE('',*,*,#1152,.T.);
#1536=ORIENTED_EDGE('',*,*,#1153,.F.);
#1537=ORIENTED_EDGE('',*,*,#1152,.F.);
#1538=ORIENTED_EDGE('',*,*,#1154,.F.);
#1539=ORIENTED_EDGE('',*,*,#1155,.F.);
#1540=ORIENTED_EDGE('',*,*,#1156,.F.);
#1541=ORIENTED_EDGE('',*,*,#1157,.T.);
#1542=ORIENTED_EDGE('',*,*,#1154,.T.);
#1543=ORIENTED_EDGE('',*,*,#1151,.F.);
#1544=ORIENTED_EDGE('',*,*,#1158,.F.);
#1545=ORIENTED_EDGE('',*,*,#1155,.T.);
#1546=ORIENTED_EDGE('',*,*,#1157,.F.);
#1547=ORIENTED_EDGE('',*,*,#1159,.T.);
#1548=ORIENTED_EDGE('',*,*,#1160,.F.);
#1549=ORIENTED_EDGE('',*,*,#1161,.T.);
#1550=ORIENTED_EDGE('',*,*,#1162,.T.);
#1551=ORIENTED_EDGE('',*,*,#1163,.T.);
#1552=ORIENTED_EDGE('',*,*,#1164,.F.);
#1553=ORIENTED_EDGE('',*,*,#1163,.F.);
#1554=ORIENTED_EDGE('',*,*,#1165,.F.);
#1555=ORIENTED_EDGE('',*,*,#1166,.F.);
#1556=ORIENTED_EDGE('',*,*,#1167,.F.);
#1557=ORIENTED_EDGE('',*,*,#1168,.T.);
#1558=ORIENTED_EDGE('',*,*,#1165,.T.);
#1559=ORIENTED_EDGE('',*,*,#1162,.F.);
#1560=ORIENTED_EDGE('',*,*,#1169,.F.);
#1561=ORIENTED_EDGE('',*,*,#1166,.T.);
#1562=ORIENTED_EDGE('',*,*,#1168,.F.);
#1563=ORIENTED_EDGE('',*,*,#1170,.T.);
#1564=ORIENTED_EDGE('',*,*,#1171,.F.);
#1565=ORIENTED_EDGE('',*,*,#1172,.T.);
#1566=ORIENTED_EDGE('',*,*,#1173,.T.);
#1567=ORIENTED_EDGE('',*,*,#1174,.T.);
#1568=ORIENTED_EDGE('',*,*,#1175,.F.);
#1569=ORIENTED_EDGE('',*,*,#1174,.F.);
#1570=ORIENTED_EDGE('',*,*,#1176,.F.);
#1571=ORIENTED_EDGE('',*,*,#1177,.F.);
#1572=ORIENTED_EDGE('',*,*,#1178,.F.);
#1573=ORIENTED_EDGE('',*,*,#1179,.T.);
#1574=ORIENTED_EDGE('',*,*,#1176,.T.);
#1575=ORIENTED_EDGE('',*,*,#1173,.F.);
#1576=ORIENTED_EDGE('',*,*,#1180,.F.);
#1577=ORIENTED_EDGE('',*,*,#1177,.T.);
#1578=ORIENTED_EDGE('',*,*,#1179,.F.);
#1579=ORIENTED_EDGE('',*,*,#1181,.T.);
#1580=ORIENTED_EDGE('',*,*,#1182,.F.);
#1581=ORIENTED_EDGE('',*,*,#1183,.T.);
#1582=ORIENTED_EDGE('',*,*,#1184,.T.);
#1583=ORIENTED_EDGE('',*,*,#1185,.T.);
#1584=ORIENTED_EDGE('',*,*,#1186,.F.);
#1585=ORIENTED_EDGE('',*,*,#1185,.F.);
#1586=ORIENTED_EDGE('',*,*,#1187,.F.);
#1587=ORIENTED_EDGE('',*,*,#1188,.F.);
#1588=ORIENTED_EDGE('',*,*,#1189,.F.);
#1589=ORIENTED_EDGE('',*,*,#1190,.T.);
#1590=ORIENTED_EDGE('',*,*,#1187,.T.);
#1591=ORIENTED_EDGE('',*,*,#1184,.F.);
#1592=ORIENTED_EDGE('',*,*,#1191,.F.);
#1593=ORIENTED_EDGE('',*,*,#1188,.T.);
#1594=ORIENTED_EDGE('',*,*,#1190,.F.);
#1595=ORIENTED_EDGE('',*,*,#1192,.T.);
#1596=ORIENTED_EDGE('',*,*,#1193,.F.);
#1597=ORIENTED_EDGE('',*,*,#1194,.T.);
#1598=ORIENTED_EDGE('',*,*,#1195,.T.);
#1599=ORIENTED_EDGE('',*,*,#1196,.T.);
#1600=ORIENTED_EDGE('',*,*,#1197,.F.);
#1601=ORIENTED_EDGE('',*,*,#1196,.F.);
#1602=ORIENTED_EDGE('',*,*,#1198,.F.);
#1603=ORIENTED_EDGE('',*,*,#1199,.F.);
#1604=ORIENTED_EDGE('',*,*,#1200,.F.);
#1605=ORIENTED_EDGE('',*,*,#1201,.T.);
#1606=ORIENTED_EDGE('',*,*,#1198,.T.);
#1607=ORIENTED_EDGE('',*,*,#1195,.F.);
#1608=ORIENTED_EDGE('',*,*,#1202,.F.);
#1609=ORIENTED_EDGE('',*,*,#1199,.T.);
#1610=ORIENTED_EDGE('',*,*,#1201,.F.);
#1611=ORIENTED_EDGE('',*,*,#1203,.T.);
#1612=ORIENTED_EDGE('',*,*,#1204,.F.);
#1613=ORIENTED_EDGE('',*,*,#1205,.T.);
#1614=ORIENTED_EDGE('',*,*,#1206,.T.);
#1615=ORIENTED_EDGE('',*,*,#1207,.T.);
#1616=ORIENTED_EDGE('',*,*,#1208,.F.);
#1617=ORIENTED_EDGE('',*,*,#1207,.F.);
#1618=ORIENTED_EDGE('',*,*,#1209,.F.);
#1619=ORIENTED_EDGE('',*,*,#1210,.F.);
#1620=ORIENTED_EDGE('',*,*,#1211,.F.);
#1621=ORIENTED_EDGE('',*,*,#1212,.T.);
#1622=ORIENTED_EDGE('',*,*,#1209,.T.);
#1623=ORIENTED_EDGE('',*,*,#1206,.F.);
#1624=ORIENTED_EDGE('',*,*,#1213,.F.);
#1625=ORIENTED_EDGE('',*,*,#1210,.T.);
#1626=ORIENTED_EDGE('',*,*,#1212,.F.);
#1627=ORIENTED_EDGE('',*,*,#1214,.T.);
#1628=ORIENTED_EDGE('',*,*,#1215,.F.);
#1629=ORIENTED_EDGE('',*,*,#1216,.T.);
#1630=ORIENTED_EDGE('',*,*,#1217,.T.);
#1631=ORIENTED_EDGE('',*,*,#1218,.T.);
#1632=ORIENTED_EDGE('',*,*,#1219,.F.);
#1633=ORIENTED_EDGE('',*,*,#1218,.F.);
#1634=ORIENTED_EDGE('',*,*,#1220,.F.);
#1635=ORIENTED_EDGE('',*,*,#1221,.F.);
#1636=ORIENTED_EDGE('',*,*,#1222,.F.);
#1637=ORIENTED_EDGE('',*,*,#1223,.T.);
#1638=ORIENTED_EDGE('',*,*,#1220,.T.);
#1639=ORIENTED_EDGE('',*,*,#1217,.F.);
#1640=ORIENTED_EDGE('',*,*,#1224,.F.);
#1641=ORIENTED_EDGE('',*,*,#1221,.T.);
#1642=ORIENTED_EDGE('',*,*,#1223,.F.);
#1643=ORIENTED_EDGE('',*,*,#1225,.T.);
#1644=ORIENTED_EDGE('',*,*,#1226,.F.);
#1645=ORIENTED_EDGE('',*,*,#1227,.T.);
#1646=ORIENTED_EDGE('',*,*,#1228,.T.);
#1647=ORIENTED_EDGE('',*,*,#1229,.T.);
#1648=ORIENTED_EDGE('',*,*,#1230,.F.);
#1649=ORIENTED_EDGE('',*,*,#1229,.F.);
#1650=ORIENTED_EDGE('',*,*,#1231,.F.);
#1651=ORIENTED_EDGE('',*,*,#1232,.F.);
#1652=ORIENTED_EDGE('',*,*,#1233,.F.);
#1653=ORIENTED_EDGE('',*,*,#1234,.T.);
#1654=ORIENTED_EDGE('',*,*,#1231,.T.);
#1655=ORIENTED_EDGE('',*,*,#1228,.F.);
#1656=ORIENTED_EDGE('',*,*,#1235,.F.);
#1657=ORIENTED_EDGE('',*,*,#1232,.T.);
#1658=ORIENTED_EDGE('',*,*,#1234,.F.);
#1659=ORIENTED_EDGE('',*,*,#1236,.T.);
#1660=ORIENTED_EDGE('',*,*,#1237,.F.);
#1661=ORIENTED_EDGE('',*,*,#1238,.T.);
#1662=ORIENTED_EDGE('',*,*,#1239,.T.);
#1663=ORIENTED_EDGE('',*,*,#1240,.T.);
#1664=ORIENTED_EDGE('',*,*,#1241,.F.);
#1665=ORIENTED_EDGE('',*,*,#1240,.F.);
#1666=ORIENTED_EDGE('',*,*,#1242,.F.);
#1667=ORIENTED_EDGE('',*,*,#1243,.F.);
#1668=ORIENTED_EDGE('',*,*,#1244,.F.);
#1669=ORIENTED_EDGE('',*,*,#1245,.T.);
#1670=ORIENTED_EDGE('',*,*,#1242,.T.);
#1671=ORIENTED_EDGE('',*,*,#1239,.F.);
#1672=ORIENTED_EDGE('',*,*,#1246,.F.);
#1673=ORIENTED_EDGE('',*,*,#1243,.T.);
#1674=ORIENTED_EDGE('',*,*,#1245,.F.);
#1675=ORIENTED_EDGE('',*,*,#1247,.T.);
#1676=ORIENTED_EDGE('',*,*,#1248,.F.);
#1677=ORIENTED_EDGE('',*,*,#1249,.T.);
#1678=ORIENTED_EDGE('',*,*,#1250,.T.);
#1679=ORIENTED_EDGE('',*,*,#1251,.T.);
#1680=ORIENTED_EDGE('',*,*,#1252,.F.);
#1681=ORIENTED_EDGE('',*,*,#1251,.F.);
#1682=ORIENTED_EDGE('',*,*,#1253,.F.);
#1683=ORIENTED_EDGE('',*,*,#1254,.F.);
#1684=ORIENTED_EDGE('',*,*,#1255,.F.);
#1685=ORIENTED_EDGE('',*,*,#1256,.T.);
#1686=ORIENTED_EDGE('',*,*,#1253,.T.);
#1687=ORIENTED_EDGE('',*,*,#1250,.F.);
#1688=ORIENTED_EDGE('',*,*,#1257,.F.);
#1689=ORIENTED_EDGE('',*,*,#1254,.T.);
#1690=ORIENTED_EDGE('',*,*,#1256,.F.);
#1691=ORIENTED_EDGE('',*,*,#1258,.T.);
#1692=ORIENTED_EDGE('',*,*,#1259,.F.);
#1693=ORIENTED_EDGE('',*,*,#1260,.T.);
#1694=ORIENTED_EDGE('',*,*,#1261,.T.);
#1695=ORIENTED_EDGE('',*,*,#1262,.T.);
#1696=ORIENTED_EDGE('',*,*,#1263,.F.);
#1697=ORIENTED_EDGE('',*,*,#1262,.F.);
#1698=ORIENTED_EDGE('',*,*,#1264,.F.);
#1699=ORIENTED_EDGE('',*,*,#1265,.F.);
#1700=ORIENTED_EDGE('',*,*,#1266,.F.);
#1701=ORIENTED_EDGE('',*,*,#1267,.T.);
#1702=ORIENTED_EDGE('',*,*,#1264,.T.);
#1703=ORIENTED_EDGE('',*,*,#1261,.F.);
#1704=ORIENTED_EDGE('',*,*,#1268,.F.);
#1705=ORIENTED_EDGE('',*,*,#1265,.T.);
#1706=ORIENTED_EDGE('',*,*,#1267,.F.);
#1707=ORIENTED_EDGE('',*,*,#1269,.T.);
#1708=ORIENTED_EDGE('',*,*,#1270,.F.);
#1709=ORIENTED_EDGE('',*,*,#1271,.T.);
#1710=ORIENTED_EDGE('',*,*,#1272,.T.);
#1711=ORIENTED_EDGE('',*,*,#1273,.T.);
#1712=ORIENTED_EDGE('',*,*,#1274,.F.);
#1713=ORIENTED_EDGE('',*,*,#1273,.F.);
#1714=ORIENTED_EDGE('',*,*,#1275,.F.);
#1715=ORIENTED_EDGE('',*,*,#1276,.F.);
#1716=ORIENTED_EDGE('',*,*,#1277,.F.);
#1717=ORIENTED_EDGE('',*,*,#1278,.T.);
#1718=ORIENTED_EDGE('',*,*,#1275,.T.);
#1719=ORIENTED_EDGE('',*,*,#1272,.F.);
#1720=ORIENTED_EDGE('',*,*,#1279,.F.);
#1721=ORIENTED_EDGE('',*,*,#1276,.T.);
#1722=ORIENTED_EDGE('',*,*,#1278,.F.);
#1723=ORIENTED_EDGE('',*,*,#1280,.T.);
#1724=ORIENTED_EDGE('',*,*,#1281,.T.);
#1725=ORIENTED_EDGE('',*,*,#1282,.T.);
#1726=ORIENTED_EDGE('',*,*,#1283,.T.);
#1727=ORIENTED_EDGE('',*,*,#1282,.F.);
#1728=ORIENTED_EDGE('',*,*,#1284,.T.);
#1729=ORIENTED_EDGE('',*,*,#1285,.T.);
#1730=ORIENTED_EDGE('',*,*,#1286,.F.);
#1731=ORIENTED_EDGE('',*,*,#1127,.T.);
#1732=ORIENTED_EDGE('',*,*,#1131,.T.);
#1733=ORIENTED_EDGE('',*,*,#1136,.T.);
#1734=ORIENTED_EDGE('',*,*,#1287,.F.);
#1735=ORIENTED_EDGE('',*,*,#1138,.T.);
#1736=ORIENTED_EDGE('',*,*,#1142,.T.);
#1737=ORIENTED_EDGE('',*,*,#1147,.T.);
#1738=ORIENTED_EDGE('',*,*,#1288,.F.);
#1739=ORIENTED_EDGE('',*,*,#1149,.T.);
#1740=ORIENTED_EDGE('',*,*,#1153,.T.);
#1741=ORIENTED_EDGE('',*,*,#1158,.T.);
#1742=ORIENTED_EDGE('',*,*,#1289,.F.);
#1743=ORIENTED_EDGE('',*,*,#1160,.T.);
#1744=ORIENTED_EDGE('',*,*,#1164,.T.);
#1745=ORIENTED_EDGE('',*,*,#1169,.T.);
#1746=ORIENTED_EDGE('',*,*,#1290,.F.);
#1747=ORIENTED_EDGE('',*,*,#1171,.T.);
#1748=ORIENTED_EDGE('',*,*,#1175,.T.);
#1749=ORIENTED_EDGE('',*,*,#1180,.T.);
#1750=ORIENTED_EDGE('',*,*,#1291,.F.);
#1751=ORIENTED_EDGE('',*,*,#1182,.T.);
#1752=ORIENTED_EDGE('',*,*,#1186,.T.);
#1753=ORIENTED_EDGE('',*,*,#1191,.T.);
#1754=ORIENTED_EDGE('',*,*,#1292,.F.);
#1755=ORIENTED_EDGE('',*,*,#1193,.T.);
#1756=ORIENTED_EDGE('',*,*,#1197,.T.);
#1757=ORIENTED_EDGE('',*,*,#1202,.T.);
#1758=ORIENTED_EDGE('',*,*,#1293,.F.);
#1759=ORIENTED_EDGE('',*,*,#1204,.T.);
#1760=ORIENTED_EDGE('',*,*,#1208,.T.);
#1761=ORIENTED_EDGE('',*,*,#1213,.T.);
#1762=ORIENTED_EDGE('',*,*,#1294,.F.);
#1763=ORIENTED_EDGE('',*,*,#1215,.T.);
#1764=ORIENTED_EDGE('',*,*,#1219,.T.);
#1765=ORIENTED_EDGE('',*,*,#1224,.T.);
#1766=ORIENTED_EDGE('',*,*,#1295,.F.);
#1767=ORIENTED_EDGE('',*,*,#1226,.T.);
#1768=ORIENTED_EDGE('',*,*,#1230,.T.);
#1769=ORIENTED_EDGE('',*,*,#1235,.T.);
#1770=ORIENTED_EDGE('',*,*,#1296,.F.);
#1771=ORIENTED_EDGE('',*,*,#1237,.T.);
#1772=ORIENTED_EDGE('',*,*,#1241,.T.);
#1773=ORIENTED_EDGE('',*,*,#1246,.T.);
#1774=ORIENTED_EDGE('',*,*,#1297,.F.);
#1775=ORIENTED_EDGE('',*,*,#1248,.T.);
#1776=ORIENTED_EDGE('',*,*,#1252,.T.);
#1777=ORIENTED_EDGE('',*,*,#1257,.T.);
#1778=ORIENTED_EDGE('',*,*,#1298,.F.);
#1779=ORIENTED_EDGE('',*,*,#1259,.T.);
#1780=ORIENTED_EDGE('',*,*,#1263,.T.);
#1781=ORIENTED_EDGE('',*,*,#1268,.T.);
#1782=ORIENTED_EDGE('',*,*,#1299,.F.);
#1783=ORIENTED_EDGE('',*,*,#1270,.T.);
#1784=ORIENTED_EDGE('',*,*,#1274,.T.);
#1785=ORIENTED_EDGE('',*,*,#1279,.T.);
#1786=ORIENTED_EDGE('',*,*,#1300,.F.);
#1787=ORIENTED_EDGE('',*,*,#1301,.T.);
#1788=ORIENTED_EDGE('',*,*,#1301,.F.);
#1789=ORIENTED_EDGE('',*,*,#1302,.T.);
#1790=ORIENTED_EDGE('',*,*,#1303,.T.);
#1791=ORIENTED_EDGE('',*,*,#1304,.T.);
#1792=ORIENTED_EDGE('',*,*,#1281,.F.);
#1793=ORIENTED_EDGE('',*,*,#1304,.F.);
#1794=ORIENTED_EDGE('',*,*,#1305,.F.);
#1795=ORIENTED_EDGE('',*,*,#1306,.F.);
#1796=ORIENTED_EDGE('',*,*,#1284,.F.);
#1797=ORIENTED_EDGE('',*,*,#1307,.F.);
#1798=ORIENTED_EDGE('',*,*,#1308,.T.);
#1799=ORIENTED_EDGE('',*,*,#1305,.T.);
#1800=ORIENTED_EDGE('',*,*,#1303,.F.);
#1801=ORIENTED_EDGE('',*,*,#1285,.F.);
#1802=ORIENTED_EDGE('',*,*,#1306,.T.);
#1803=ORIENTED_EDGE('',*,*,#1308,.F.);
#1804=ORIENTED_EDGE('',*,*,#1309,.T.);
#1805=ORIENTED_EDGE('',*,*,#1310,.T.);
#1806=ORIENTED_EDGE('',*,*,#1283,.F.);
#1807=ORIENTED_EDGE('',*,*,#1311,.F.);
#1808=ORIENTED_EDGE('',*,*,#1286,.T.);
#1809=ORIENTED_EDGE('',*,*,#1309,.F.);
#1810=ORIENTED_EDGE('',*,*,#1307,.T.);
#1811=ORIENTED_EDGE('',*,*,#1302,.F.);
#1812=ORIENTED_EDGE('',*,*,#1300,.T.);
#1813=ORIENTED_EDGE('',*,*,#1280,.F.);
#1814=ORIENTED_EDGE('',*,*,#1277,.T.);
#1815=ORIENTED_EDGE('',*,*,#1271,.F.);
#1816=ORIENTED_EDGE('',*,*,#1299,.T.);
#1817=ORIENTED_EDGE('',*,*,#1269,.F.);
#1818=ORIENTED_EDGE('',*,*,#1266,.T.);
#1819=ORIENTED_EDGE('',*,*,#1260,.F.);
#1820=ORIENTED_EDGE('',*,*,#1298,.T.);
#1821=ORIENTED_EDGE('',*,*,#1258,.F.);
#1822=ORIENTED_EDGE('',*,*,#1255,.T.);
#1823=ORIENTED_EDGE('',*,*,#1249,.F.);
#1824=ORIENTED_EDGE('',*,*,#1297,.T.);
#1825=ORIENTED_EDGE('',*,*,#1247,.F.);
#1826=ORIENTED_EDGE('',*,*,#1244,.T.);
#1827=ORIENTED_EDGE('',*,*,#1238,.F.);
#1828=ORIENTED_EDGE('',*,*,#1296,.T.);
#1829=ORIENTED_EDGE('',*,*,#1236,.F.);
#1830=ORIENTED_EDGE('',*,*,#1233,.T.);
#1831=ORIENTED_EDGE('',*,*,#1227,.F.);
#1832=ORIENTED_EDGE('',*,*,#1295,.T.);
#1833=ORIENTED_EDGE('',*,*,#1225,.F.);
#1834=ORIENTED_EDGE('',*,*,#1222,.T.);
#1835=ORIENTED_EDGE('',*,*,#1216,.F.);
#1836=ORIENTED_EDGE('',*,*,#1294,.T.);
#1837=ORIENTED_EDGE('',*,*,#1214,.F.);
#1838=ORIENTED_EDGE('',*,*,#1211,.T.);
#1839=ORIENTED_EDGE('',*,*,#1205,.F.);
#1840=ORIENTED_EDGE('',*,*,#1293,.T.);
#1841=ORIENTED_EDGE('',*,*,#1203,.F.);
#1842=ORIENTED_EDGE('',*,*,#1200,.T.);
#1843=ORIENTED_EDGE('',*,*,#1194,.F.);
#1844=ORIENTED_EDGE('',*,*,#1292,.T.);
#1845=ORIENTED_EDGE('',*,*,#1192,.F.);
#1846=ORIENTED_EDGE('',*,*,#1189,.T.);
#1847=ORIENTED_EDGE('',*,*,#1183,.F.);
#1848=ORIENTED_EDGE('',*,*,#1291,.T.);
#1849=ORIENTED_EDGE('',*,*,#1181,.F.);
#1850=ORIENTED_EDGE('',*,*,#1178,.T.);
#1851=ORIENTED_EDGE('',*,*,#1172,.F.);
#1852=ORIENTED_EDGE('',*,*,#1290,.T.);
#1853=ORIENTED_EDGE('',*,*,#1170,.F.);
#1854=ORIENTED_EDGE('',*,*,#1167,.T.);
#1855=ORIENTED_EDGE('',*,*,#1161,.F.);
#1856=ORIENTED_EDGE('',*,*,#1289,.T.);
#1857=ORIENTED_EDGE('',*,*,#1159,.F.);
#1858=ORIENTED_EDGE('',*,*,#1156,.T.);
#1859=ORIENTED_EDGE('',*,*,#1150,.F.);
#1860=ORIENTED_EDGE('',*,*,#1288,.T.);
#1861=ORIENTED_EDGE('',*,*,#1148,.F.);
#1862=ORIENTED_EDGE('',*,*,#1145,.T.);
#1863=ORIENTED_EDGE('',*,*,#1139,.F.);
#1864=ORIENTED_EDGE('',*,*,#1287,.T.);
#1865=ORIENTED_EDGE('',*,*,#1137,.F.);
#1866=ORIENTED_EDGE('',*,*,#1134,.T.);
#1867=ORIENTED_EDGE('',*,*,#1128,.F.);
#1868=ORIENTED_EDGE('',*,*,#1312,.F.);
#1869=ORIENTED_EDGE('',*,*,#1313,.T.);
#1870=ORIENTED_EDGE('',*,*,#1311,.T.);
#1871=ORIENTED_EDGE('',*,*,#1313,.F.);
#1872=ORIENTED_EDGE('',*,*,#1314,.F.);
#1873=ORIENTED_EDGE('',*,*,#1315,.T.);
#1874=ORIENTED_EDGE('',*,*,#1124,.T.);
#1875=ORIENTED_EDGE('',*,*,#1126,.T.);
#1876=ORIENTED_EDGE('',*,*,#1316,.T.);
#1877=ORIENTED_EDGE('',*,*,#1312,.T.);
#1878=ORIENTED_EDGE('',*,*,#1316,.F.);
#1879=ORIENTED_EDGE('',*,*,#1125,.T.);
#1880=ORIENTED_EDGE('',*,*,#1315,.F.);
#1881=ORIENTED_EDGE('',*,*,#1113,.T.);
#1882=ORIENTED_EDGE('',*,*,#1114,.T.);
#1883=ORIENTED_EDGE('',*,*,#1314,.T.);
#1884=ORIENTED_EDGE('',*,*,#1317,.T.);
#1885=ORIENTED_EDGE('',*,*,#1318,.F.);
#1886=ORIENTED_EDGE('',*,*,#1317,.F.);
#1887=ORIENTED_EDGE('',*,*,#1318,.T.);
#1888=ORIENTED_EDGE('',*,*,#1319,.F.);
#1889=ORIENTED_EDGE('',*,*,#1320,.F.);
#1890=ORIENTED_EDGE('',*,*,#1321,.T.);
#1891=ORIENTED_EDGE('',*,*,#1319,.T.);
#1892=ORIENTED_EDGE('',*,*,#1321,.F.);
#1893=ORIENTED_EDGE('',*,*,#1320,.T.);
#1894=ORIENTED_EDGE('',*,*,#1322,.T.);
#1895=ORIENTED_EDGE('',*,*,#1323,.F.);
#1896=ORIENTED_EDGE('',*,*,#1322,.F.);
#1897=ORIENTED_EDGE('',*,*,#1323,.T.);
#1898=ORIENTED_EDGE('',*,*,#1324,.F.);
#1899=ORIENTED_EDGE('',*,*,#1120,.F.);
#1900=ORIENTED_EDGE('',*,*,#1325,.T.);
#1901=ORIENTED_EDGE('',*,*,#1324,.T.);
#1902=ORIENTED_EDGE('',*,*,#1325,.F.);
#1903=ORIENTED_EDGE('',*,*,#1115,.T.);
#1904=ORIENTED_EDGE('',*,*,#1326,.T.);
#1905=ORIENTED_EDGE('',*,*,#1327,.F.);
#1906=ORIENTED_EDGE('',*,*,#1326,.F.);
#1907=ORIENTED_EDGE('',*,*,#1328,.F.);
#1908=ORIENTED_EDGE('',*,*,#1327,.T.);
#1909=ORIENTED_EDGE('',*,*,#1329,.F.);
#1910=ORIENTED_EDGE('',*,*,#1330,.T.);
#1911=ORIENTED_EDGE('',*,*,#1328,.T.);
#1912=ORIENTED_EDGE('',*,*,#1330,.F.);
#1913=ORIENTED_EDGE('',*,*,#1329,.T.);
#1914=ORIENTED_EDGE('',*,*,#1331,.T.);
#1915=ORIENTED_EDGE('',*,*,#1332,.F.);
#1916=ORIENTED_EDGE('',*,*,#1331,.F.);
#1917=ORIENTED_EDGE('',*,*,#1333,.F.);
#1918=ORIENTED_EDGE('',*,*,#1332,.T.);
#1919=ORIENTED_EDGE('',*,*,#1334,.F.);
#1920=ORIENTED_EDGE('',*,*,#1335,.T.);
#1921=ORIENTED_EDGE('',*,*,#1333,.T.);
#1922=ORIENTED_EDGE('',*,*,#1335,.F.);
#1923=ORIENTED_EDGE('',*,*,#1336,.F.);
#1924=ORIENTED_EDGE('',*,*,#1337,.T.);
#1925=ORIENTED_EDGE('',*,*,#1334,.T.);
#1926=ORIENTED_EDGE('',*,*,#1337,.F.);
#1927=ORIENTED_EDGE('',*,*,#1336,.T.);
#1928=ORIENTED_EDGE('',*,*,#1338,.T.);
#1929=ORIENTED_EDGE('',*,*,#1310,.F.);
#1930=ORIENTED_EDGE('',*,*,#1338,.F.);
#1931=ORIENTED_EDGE('',*,*,#1339,.F.);
#1932=ORIENTED_EDGE('',*,*,#1340,.F.);
#1933=ORIENTED_EDGE('',*,*,#1341,.F.);
#1934=ORIENTED_EDGE('',*,*,#1342,.T.);
#1935=ORIENTED_EDGE('',*,*,#1343,.F.);
#1936=ORIENTED_EDGE('',*,*,#1344,.F.);
#1937=ORIENTED_EDGE('',*,*,#1339,.T.);
#1938=ORIENTED_EDGE('',*,*,#1345,.T.);
#1939=ORIENTED_EDGE('',*,*,#1346,.F.);
#1940=ORIENTED_EDGE('',*,*,#1347,.F.);
#1941=ORIENTED_EDGE('',*,*,#1343,.T.);
#1942=ORIENTED_EDGE('',*,*,#1348,.T.);
#1943=ORIENTED_EDGE('',*,*,#1349,.F.);
#1944=ORIENTED_EDGE('',*,*,#1350,.F.);
#1945=ORIENTED_EDGE('',*,*,#1346,.T.);
#1946=ORIENTED_EDGE('',*,*,#1351,.T.);
#1947=ORIENTED_EDGE('',*,*,#1352,.F.);
#1948=ORIENTED_EDGE('',*,*,#1353,.F.);
#1949=ORIENTED_EDGE('',*,*,#1349,.T.);
#1950=ORIENTED_EDGE('',*,*,#1354,.T.);
#1951=ORIENTED_EDGE('',*,*,#1355,.F.);
#1952=ORIENTED_EDGE('',*,*,#1356,.F.);
#1953=ORIENTED_EDGE('',*,*,#1352,.T.);
#1954=ORIENTED_EDGE('',*,*,#1357,.T.);
#1955=ORIENTED_EDGE('',*,*,#1358,.F.);
#1956=ORIENTED_EDGE('',*,*,#1359,.T.);
#1957=ORIENTED_EDGE('',*,*,#1360,.T.);
#1958=ORIENTED_EDGE('',*,*,#1361,.T.);
#1959=ORIENTED_EDGE('',*,*,#1362,.F.);
#1960=ORIENTED_EDGE('',*,*,#1363,.T.);
#1961=ORIENTED_EDGE('',*,*,#1358,.T.);
#1962=ORIENTED_EDGE('',*,*,#1364,.T.);
#1963=ORIENTED_EDGE('',*,*,#1365,.F.);
#1964=ORIENTED_EDGE('',*,*,#1366,.T.);
#1965=ORIENTED_EDGE('',*,*,#1362,.T.);
#1966=ORIENTED_EDGE('',*,*,#1367,.T.);
#1967=ORIENTED_EDGE('',*,*,#1368,.F.);
#1968=ORIENTED_EDGE('',*,*,#1369,.T.);
#1969=ORIENTED_EDGE('',*,*,#1365,.T.);
#1970=ORIENTED_EDGE('',*,*,#1370,.T.);
#1971=ORIENTED_EDGE('',*,*,#1371,.F.);
#1972=ORIENTED_EDGE('',*,*,#1372,.T.);
#1973=ORIENTED_EDGE('',*,*,#1368,.T.);
#1974=ORIENTED_EDGE('',*,*,#1373,.T.);
#1975=ORIENTED_EDGE('',*,*,#1374,.F.);
#1976=ORIENTED_EDGE('',*,*,#1375,.T.);
#1977=ORIENTED_EDGE('',*,*,#1371,.T.);
#1978=ORIENTED_EDGE('',*,*,#1376,.T.);
#1979=ORIENTED_EDGE('',*,*,#1374,.T.);
#1980=ORIENTED_EDGE('',*,*,#1377,.T.);
#1981=ORIENTED_EDGE('',*,*,#1378,.F.);
#1982=ORIENTED_EDGE('',*,*,#1379,.T.);
#1983=ORIENTED_EDGE('',*,*,#1355,.T.);
#1984=ORIENTED_EDGE('',*,*,#1380,.T.);
#1985=ORIENTED_EDGE('',*,*,#1381,.F.);
#1986=ORIENTED_EDGE('',*,*,#1382,.F.);
#1987=ORIENTED_EDGE('',*,*,#1383,.F.);
#1988=ORIENTED_EDGE('',*,*,#1377,.F.);
#1989=ORIENTED_EDGE('',*,*,#1376,.F.);
#1990=ORIENTED_EDGE('',*,*,#1373,.F.);
#1991=ORIENTED_EDGE('',*,*,#1370,.F.);
#1992=ORIENTED_EDGE('',*,*,#1367,.F.);
#1993=ORIENTED_EDGE('',*,*,#1364,.F.);
#1994=ORIENTED_EDGE('',*,*,#1361,.F.);
#1995=ORIENTED_EDGE('',*,*,#1384,.F.);
#1996=ORIENTED_EDGE('',*,*,#1340,.T.);
#1997=ORIENTED_EDGE('',*,*,#1344,.T.);
#1998=ORIENTED_EDGE('',*,*,#1347,.T.);
#1999=ORIENTED_EDGE('',*,*,#1350,.T.);
#2000=ORIENTED_EDGE('',*,*,#1353,.T.);
#2001=ORIENTED_EDGE('',*,*,#1356,.T.);
#2002=ORIENTED_EDGE('',*,*,#1382,.T.);
#2003=ORIENTED_EDGE('',*,*,#1385,.F.);
#2004=ORIENTED_EDGE('',*,*,#1380,.F.);
#2005=ORIENTED_EDGE('',*,*,#1357,.F.);
#2006=ORIENTED_EDGE('',*,*,#1354,.F.);
#2007=ORIENTED_EDGE('',*,*,#1351,.F.);
#2008=ORIENTED_EDGE('',*,*,#1348,.F.);
#2009=ORIENTED_EDGE('',*,*,#1345,.F.);
#2010=ORIENTED_EDGE('',*,*,#1342,.F.);
#2011=ORIENTED_EDGE('',*,*,#1386,.F.);
#2012=ORIENTED_EDGE('',*,*,#1359,.F.);
#2013=ORIENTED_EDGE('',*,*,#1363,.F.);
#2014=ORIENTED_EDGE('',*,*,#1366,.F.);
#2015=ORIENTED_EDGE('',*,*,#1369,.F.);
#2016=ORIENTED_EDGE('',*,*,#1372,.F.);
#2017=ORIENTED_EDGE('',*,*,#1375,.F.);
#2018=ORIENTED_EDGE('',*,*,#1379,.F.);
#2019=ORIENTED_EDGE('',*,*,#1383,.T.);
#2020=ORIENTED_EDGE('',*,*,#1381,.T.);
#2021=ORIENTED_EDGE('',*,*,#1385,.T.);
#2022=ORIENTED_EDGE('',*,*,#1378,.T.);
#2023=ORIENTED_EDGE('',*,*,#1387,.T.);
#2024=ORIENTED_EDGE('',*,*,#1388,.T.);
#2025=ORIENTED_EDGE('',*,*,#1389,.T.);
#2026=ORIENTED_EDGE('',*,*,#1390,.T.);
#2027=ORIENTED_EDGE('',*,*,#1391,.T.);
#2028=ORIENTED_EDGE('',*,*,#1392,.T.);
#2029=ORIENTED_EDGE('',*,*,#1387,.F.);
#2030=ORIENTED_EDGE('',*,*,#1393,.T.);
#2031=ORIENTED_EDGE('',*,*,#1394,.T.);
#2032=ORIENTED_EDGE('',*,*,#1395,.F.);
#2033=ORIENTED_EDGE('',*,*,#1392,.F.);
#2034=ORIENTED_EDGE('',*,*,#1396,.T.);
#2035=ORIENTED_EDGE('',*,*,#1397,.T.);
#2036=ORIENTED_EDGE('',*,*,#1393,.F.);
#2037=ORIENTED_EDGE('',*,*,#1391,.F.);
#2038=ORIENTED_EDGE('',*,*,#1398,.T.);
#2039=ORIENTED_EDGE('',*,*,#1399,.T.);
#2040=ORIENTED_EDGE('',*,*,#1396,.F.);
#2041=ORIENTED_EDGE('',*,*,#1390,.F.);
#2042=ORIENTED_EDGE('',*,*,#1400,.T.);
#2043=ORIENTED_EDGE('',*,*,#1401,.T.);
#2044=ORIENTED_EDGE('',*,*,#1398,.F.);
#2045=ORIENTED_EDGE('',*,*,#1389,.F.);
#2046=ORIENTED_EDGE('',*,*,#1402,.T.);
#2047=ORIENTED_EDGE('',*,*,#1403,.T.);
#2048=ORIENTED_EDGE('',*,*,#1400,.F.);
#2049=ORIENTED_EDGE('',*,*,#1388,.F.);
#2050=ORIENTED_EDGE('',*,*,#1395,.T.);
#2051=ORIENTED_EDGE('',*,*,#1404,.T.);
#2052=ORIENTED_EDGE('',*,*,#1402,.F.);
#2053=ORIENTED_EDGE('',*,*,#1404,.F.);
#2054=ORIENTED_EDGE('',*,*,#1394,.F.);
#2055=ORIENTED_EDGE('',*,*,#1397,.F.);
#2056=ORIENTED_EDGE('',*,*,#1399,.F.);
#2057=ORIENTED_EDGE('',*,*,#1401,.F.);
#2058=ORIENTED_EDGE('',*,*,#1403,.F.);
#2059=ORIENTED_EDGE('',*,*,#1384,.T.);
#2060=ORIENTED_EDGE('',*,*,#1360,.F.);
#2061=ORIENTED_EDGE('',*,*,#1386,.T.);
#2062=ORIENTED_EDGE('',*,*,#1341,.T.);
#2063=ORIENTED_EDGE('',*,*,#1405,.F.);
#2064=ORIENTED_EDGE('',*,*,#1406,.F.);
#2065=ORIENTED_EDGE('',*,*,#1407,.F.);
#2066=ORIENTED_EDGE('',*,*,#1408,.T.);
#2067=ORIENTED_EDGE('',*,*,#1409,.F.);
#2068=ORIENTED_EDGE('',*,*,#1410,.F.);
#2069=ORIENTED_EDGE('',*,*,#1405,.T.);
#2070=ORIENTED_EDGE('',*,*,#1411,.T.);
#2071=ORIENTED_EDGE('',*,*,#1412,.F.);
#2072=ORIENTED_EDGE('',*,*,#1413,.F.);
#2073=ORIENTED_EDGE('',*,*,#1409,.T.);
#2074=ORIENTED_EDGE('',*,*,#1414,.T.);
#2075=ORIENTED_EDGE('',*,*,#1415,.F.);
#2076=ORIENTED_EDGE('',*,*,#1416,.F.);
#2077=ORIENTED_EDGE('',*,*,#1412,.T.);
#2078=ORIENTED_EDGE('',*,*,#1417,.T.);
#2079=ORIENTED_EDGE('',*,*,#1418,.F.);
#2080=ORIENTED_EDGE('',*,*,#1419,.F.);
#2081=ORIENTED_EDGE('',*,*,#1415,.T.);
#2082=ORIENTED_EDGE('',*,*,#1420,.T.);
#2083=ORIENTED_EDGE('',*,*,#1421,.F.);
#2084=ORIENTED_EDGE('',*,*,#1422,.F.);
#2085=ORIENTED_EDGE('',*,*,#1418,.T.);
#2086=ORIENTED_EDGE('',*,*,#1423,.T.);
#2087=ORIENTED_EDGE('',*,*,#1424,.F.);
#2088=ORIENTED_EDGE('',*,*,#1425,.T.);
#2089=ORIENTED_EDGE('',*,*,#1426,.T.);
#2090=ORIENTED_EDGE('',*,*,#1427,.T.);
#2091=ORIENTED_EDGE('',*,*,#1428,.F.);
#2092=ORIENTED_EDGE('',*,*,#1429,.T.);
#2093=ORIENTED_EDGE('',*,*,#1424,.T.);
#2094=ORIENTED_EDGE('',*,*,#1430,.T.);
#2095=ORIENTED_EDGE('',*,*,#1431,.F.);
#2096=ORIENTED_EDGE('',*,*,#1432,.T.);
#2097=ORIENTED_EDGE('',*,*,#1428,.T.);
#2098=ORIENTED_EDGE('',*,*,#1433,.T.);
#2099=ORIENTED_EDGE('',*,*,#1434,.F.);
#2100=ORIENTED_EDGE('',*,*,#1435,.T.);
#2101=ORIENTED_EDGE('',*,*,#1431,.T.);
#2102=ORIENTED_EDGE('',*,*,#1436,.T.);
#2103=ORIENTED_EDGE('',*,*,#1437,.F.);
#2104=ORIENTED_EDGE('',*,*,#1438,.T.);
#2105=ORIENTED_EDGE('',*,*,#1434,.T.);
#2106=ORIENTED_EDGE('',*,*,#1439,.T.);
#2107=ORIENTED_EDGE('',*,*,#1440,.F.);
#2108=ORIENTED_EDGE('',*,*,#1441,.T.);
#2109=ORIENTED_EDGE('',*,*,#1437,.T.);
#2110=ORIENTED_EDGE('',*,*,#1442,.T.);
#2111=ORIENTED_EDGE('',*,*,#1440,.T.);
#2112=ORIENTED_EDGE('',*,*,#1443,.T.);
#2113=ORIENTED_EDGE('',*,*,#1444,.F.);
#2114=ORIENTED_EDGE('',*,*,#1445,.T.);
#2115=ORIENTED_EDGE('',*,*,#1421,.T.);
#2116=ORIENTED_EDGE('',*,*,#1446,.T.);
#2117=ORIENTED_EDGE('',*,*,#1447,.F.);
#2118=ORIENTED_EDGE('',*,*,#1448,.F.);
#2119=ORIENTED_EDGE('',*,*,#1449,.F.);
#2120=ORIENTED_EDGE('',*,*,#1443,.F.);
#2121=ORIENTED_EDGE('',*,*,#1442,.F.);
#2122=ORIENTED_EDGE('',*,*,#1439,.F.);
#2123=ORIENTED_EDGE('',*,*,#1436,.F.);
#2124=ORIENTED_EDGE('',*,*,#1433,.F.);
#2125=ORIENTED_EDGE('',*,*,#1430,.F.);
#2126=ORIENTED_EDGE('',*,*,#1427,.F.);
#2127=ORIENTED_EDGE('',*,*,#1450,.F.);
#2128=ORIENTED_EDGE('',*,*,#1406,.T.);
#2129=ORIENTED_EDGE('',*,*,#1410,.T.);
#2130=ORIENTED_EDGE('',*,*,#1413,.T.);
#2131=ORIENTED_EDGE('',*,*,#1416,.T.);
#2132=ORIENTED_EDGE('',*,*,#1419,.T.);
#2133=ORIENTED_EDGE('',*,*,#1422,.T.);
#2134=ORIENTED_EDGE('',*,*,#1448,.T.);
#2135=ORIENTED_EDGE('',*,*,#1451,.F.);
#2136=ORIENTED_EDGE('',*,*,#1446,.F.);
#2137=ORIENTED_EDGE('',*,*,#1423,.F.);
#2138=ORIENTED_EDGE('',*,*,#1420,.F.);
#2139=ORIENTED_EDGE('',*,*,#1417,.F.);
#2140=ORIENTED_EDGE('',*,*,#1414,.F.);
#2141=ORIENTED_EDGE('',*,*,#1411,.F.);
#2142=ORIENTED_EDGE('',*,*,#1408,.F.);
#2143=ORIENTED_EDGE('',*,*,#1452,.F.);
#2144=ORIENTED_EDGE('',*,*,#1425,.F.);
#2145=ORIENTED_EDGE('',*,*,#1429,.F.);
#2146=ORIENTED_EDGE('',*,*,#1432,.F.);
#2147=ORIENTED_EDGE('',*,*,#1435,.F.);
#2148=ORIENTED_EDGE('',*,*,#1438,.F.);
#2149=ORIENTED_EDGE('',*,*,#1441,.F.);
#2150=ORIENTED_EDGE('',*,*,#1445,.F.);
#2151=ORIENTED_EDGE('',*,*,#1449,.T.);
#2152=ORIENTED_EDGE('',*,*,#1447,.T.);
#2153=ORIENTED_EDGE('',*,*,#1451,.T.);
#2154=ORIENTED_EDGE('',*,*,#1444,.T.);
#2155=ORIENTED_EDGE('',*,*,#1453,.T.);
#2156=ORIENTED_EDGE('',*,*,#1454,.T.);
#2157=ORIENTED_EDGE('',*,*,#1455,.T.);
#2158=ORIENTED_EDGE('',*,*,#1456,.T.);
#2159=ORIENTED_EDGE('',*,*,#1457,.T.);
#2160=ORIENTED_EDGE('',*,*,#1458,.T.);
#2161=ORIENTED_EDGE('',*,*,#1453,.F.);
#2162=ORIENTED_EDGE('',*,*,#1459,.T.);
#2163=ORIENTED_EDGE('',*,*,#1460,.T.);
#2164=ORIENTED_EDGE('',*,*,#1461,.F.);
#2165=ORIENTED_EDGE('',*,*,#1458,.F.);
#2166=ORIENTED_EDGE('',*,*,#1462,.T.);
#2167=ORIENTED_EDGE('',*,*,#1463,.T.);
#2168=ORIENTED_EDGE('',*,*,#1459,.F.);
#2169=ORIENTED_EDGE('',*,*,#1457,.F.);
#2170=ORIENTED_EDGE('',*,*,#1464,.T.);
#2171=ORIENTED_EDGE('',*,*,#1465,.T.);
#2172=ORIENTED_EDGE('',*,*,#1462,.F.);
#2173=ORIENTED_EDGE('',*,*,#1456,.F.);
#2174=ORIENTED_EDGE('',*,*,#1466,.T.);
#2175=ORIENTED_EDGE('',*,*,#1467,.T.);
#2176=ORIENTED_EDGE('',*,*,#1464,.F.);
#2177=ORIENTED_EDGE('',*,*,#1455,.F.);
#2178=ORIENTED_EDGE('',*,*,#1468,.T.);
#2179=ORIENTED_EDGE('',*,*,#1469,.T.);
#2180=ORIENTED_EDGE('',*,*,#1466,.F.);
#2181=ORIENTED_EDGE('',*,*,#1454,.F.);
#2182=ORIENTED_EDGE('',*,*,#1461,.T.);
#2183=ORIENTED_EDGE('',*,*,#1470,.T.);
#2184=ORIENTED_EDGE('',*,*,#1468,.F.);
#2185=ORIENTED_EDGE('',*,*,#1470,.F.);
#2186=ORIENTED_EDGE('',*,*,#1460,.F.);
#2187=ORIENTED_EDGE('',*,*,#1463,.F.);
#2188=ORIENTED_EDGE('',*,*,#1465,.F.);
#2189=ORIENTED_EDGE('',*,*,#1467,.F.);
#2190=ORIENTED_EDGE('',*,*,#1469,.F.);
#2191=ORIENTED_EDGE('',*,*,#1450,.T.);
#2192=ORIENTED_EDGE('',*,*,#1426,.F.);
#2193=ORIENTED_EDGE('',*,*,#1452,.T.);
#2194=ORIENTED_EDGE('',*,*,#1407,.T.);
#2195=CYLINDRICAL_SURFACE('',#2445,2.00054127207588);
#2196=CYLINDRICAL_SURFACE('',#2446,2.50080065552765);
#2197=CYLINDRICAL_SURFACE('',#2449,2.00007126058529);
#2198=CYLINDRICAL_SURFACE('',#2450,0.124032861755453);
#2199=CYLINDRICAL_SURFACE('',#2457,0.749041401963156);
#2200=CYLINDRICAL_SURFACE('',#2459,0.124032861755453);
#2201=CYLINDRICAL_SURFACE('',#2461,0.124032861755453);
#2202=CYLINDRICAL_SURFACE('',#2468,0.749041401963156);
#2203=CYLINDRICAL_SURFACE('',#2470,0.124032861755453);
#2204=CYLINDRICAL_SURFACE('',#2472,0.124032861755453);
#2205=CYLINDRICAL_SURFACE('',#2479,0.749041401963155);
#2206=CYLINDRICAL_SURFACE('',#2481,0.124032861755453);
#2207=CYLINDRICAL_SURFACE('',#2483,0.124032861755453);
#2208=CYLINDRICAL_SURFACE('',#2490,0.749041401963156);
#2209=CYLINDRICAL_SURFACE('',#2492,0.124032861755453);
#2210=CYLINDRICAL_SURFACE('',#2494,0.124032861755453);
#2211=CYLINDRICAL_SURFACE('',#2501,0.749041401963155);
#2212=CYLINDRICAL_SURFACE('',#2503,0.124032861755453);
#2213=CYLINDRICAL_SURFACE('',#2505,0.124032861755453);
#2214=CYLINDRICAL_SURFACE('',#2512,0.749041401963156);
#2215=CYLINDRICAL_SURFACE('',#2514,0.124032861755453);
#2216=CYLINDRICAL_SURFACE('',#2516,0.124032861755453);
#2217=CYLINDRICAL_SURFACE('',#2523,0.749041401963155);
#2218=CYLINDRICAL_SURFACE('',#2525,0.124032861755453);
#2219=CYLINDRICAL_SURFACE('',#2527,0.124032861755453);
#2220=CYLINDRICAL_SURFACE('',#2534,0.749041401963156);
#2221=CYLINDRICAL_SURFACE('',#2536,0.124032861755453);
#2222=CYLINDRICAL_SURFACE('',#2538,0.124032861755453);
#2223=CYLINDRICAL_SURFACE('',#2545,0.749041401963155);
#2224=CYLINDRICAL_SURFACE('',#2547,0.124032861755453);
#2225=CYLINDRICAL_SURFACE('',#2549,0.124032861755453);
#2226=CYLINDRICAL_SURFACE('',#2556,0.749041401963156);
#2227=CYLINDRICAL_SURFACE('',#2558,0.124032861755453);
#2228=CYLINDRICAL_SURFACE('',#2560,0.124032861755453);
#2229=CYLINDRICAL_SURFACE('',#2567,0.749041401963156);
#2230=CYLINDRICAL_SURFACE('',#2569,0.124032861755453);
#2231=CYLINDRICAL_SURFACE('',#2571,0.124032861755453);
#2232=CYLINDRICAL_SURFACE('',#2578,0.749041401963155);
#2233=CYLINDRICAL_SURFACE('',#2580,0.124032861755453);
#2234=CYLINDRICAL_SURFACE('',#2582,0.124032861755453);
#2235=CYLINDRICAL_SURFACE('',#2589,0.749041401963156);
#2236=CYLINDRICAL_SURFACE('',#2591,0.124032861755453);
#2237=CYLINDRICAL_SURFACE('',#2593,0.124032861755453);
#2238=CYLINDRICAL_SURFACE('',#2600,0.749041401963155);
#2239=CYLINDRICAL_SURFACE('',#2602,0.124032861755453);
#2240=CYLINDRICAL_SURFACE('',#2604,4.75930776765241);
#2241=CYLINDRICAL_SURFACE('',#2623,0.124032861755453);
#2242=CYLINDRICAL_SURFACE('',#2629,0.749041401963155);
#2243=CYLINDRICAL_SURFACE('',#2631,0.124032861755453);
#2244=CYLINDRICAL_SURFACE('',#2639,6.94701057265674);
#2245=CYLINDRICAL_SURFACE('',#2664,6.94665463816359);
#2246=CYLINDRICAL_SURFACE('',#2668,1.5555);
#2247=CYLINDRICAL_SURFACE('',#2670,1.5555);
#2248=CYLINDRICAL_SURFACE('',#2671,1.5555);
#2249=CYLINDRICAL_SURFACE('',#2672,1.5555);
#2250=CYLINDRICAL_SURFACE('',#2673,1.5555);
#2251=CYLINDRICAL_SURFACE('',#2674,1.5555);
#2252=CYLINDRICAL_SURFACE('',#2675,1.954);
#2253=CYLINDRICAL_SURFACE('',#2677,1.954);
#2254=CYLINDRICAL_SURFACE('',#2678,1.954);
#2255=CYLINDRICAL_SURFACE('',#2679,1.954);
#2256=CYLINDRICAL_SURFACE('',#2680,1.954);
#2257=CYLINDRICAL_SURFACE('',#2681,1.954);
#2258=CYLINDRICAL_SURFACE('',#2682,1.954);
#2259=CYLINDRICAL_SURFACE('',#2684,1.5555);
#2260=CYLINDRICAL_SURFACE('',#2696,1.5555);
#2261=CYLINDRICAL_SURFACE('',#2698,1.5555);
#2262=CYLINDRICAL_SURFACE('',#2699,1.5555);
#2263=CYLINDRICAL_SURFACE('',#2700,1.5555);
#2264=CYLINDRICAL_SURFACE('',#2701,1.5555);
#2265=CYLINDRICAL_SURFACE('',#2702,1.5555);
#2266=CYLINDRICAL_SURFACE('',#2703,1.954);
#2267=CYLINDRICAL_SURFACE('',#2705,1.954);
#2268=CYLINDRICAL_SURFACE('',#2706,1.954);
#2269=CYLINDRICAL_SURFACE('',#2707,1.954);
#2270=CYLINDRICAL_SURFACE('',#2708,1.954);
#2271=CYLINDRICAL_SURFACE('',#2709,1.954);
#2272=CYLINDRICAL_SURFACE('',#2710,1.954);
#2273=CYLINDRICAL_SURFACE('',#2712,1.5555);
#2274=ADVANCED_FACE('',(#245),#2195,.F.);
#2275=ADVANCED_FACE('',(#246),#2196,.F.);
#2276=ADVANCED_FACE('',(#247),#2197,.F.);
#2277=ADVANCED_FACE('',(#248),#2198,.T.);
#2278=ADVANCED_FACE('',(#249),#58,.F.);
#2279=ADVANCED_FACE('',(#250),#2199,.F.);
#2280=ADVANCED_FACE('',(#251),#2200,.T.);
#2281=ADVANCED_FACE('',(#252),#2201,.T.);
#2282=ADVANCED_FACE('',(#253),#59,.F.);
#2283=ADVANCED_FACE('',(#254),#2202,.F.);
#2284=ADVANCED_FACE('',(#255),#2203,.T.);
#2285=ADVANCED_FACE('',(#256),#2204,.T.);
#2286=ADVANCED_FACE('',(#257),#60,.F.);
#2287=ADVANCED_FACE('',(#258),#2205,.F.);
#2288=ADVANCED_FACE('',(#259),#2206,.T.);
#2289=ADVANCED_FACE('',(#260),#2207,.T.);
#2290=ADVANCED_FACE('',(#261),#61,.F.);
#2291=ADVANCED_FACE('',(#262),#2208,.F.);
#2292=ADVANCED_FACE('',(#263),#2209,.T.);
#2293=ADVANCED_FACE('',(#264),#2210,.T.);
#2294=ADVANCED_FACE('',(#265),#62,.F.);
#2295=ADVANCED_FACE('',(#266),#2211,.F.);
#2296=ADVANCED_FACE('',(#267),#2212,.T.);
#2297=ADVANCED_FACE('',(#268),#2213,.T.);
#2298=ADVANCED_FACE('',(#269),#63,.F.);
#2299=ADVANCED_FACE('',(#270),#2214,.F.);
#2300=ADVANCED_FACE('',(#271),#2215,.T.);
#2301=ADVANCED_FACE('',(#272),#2216,.T.);
#2302=ADVANCED_FACE('',(#273),#64,.F.);
#2303=ADVANCED_FACE('',(#274),#2217,.F.);
#2304=ADVANCED_FACE('',(#275),#2218,.T.);
#2305=ADVANCED_FACE('',(#276),#2219,.T.);
#2306=ADVANCED_FACE('',(#277),#65,.F.);
#2307=ADVANCED_FACE('',(#278),#2220,.F.);
#2308=ADVANCED_FACE('',(#279),#2221,.T.);
#2309=ADVANCED_FACE('',(#280),#2222,.T.);
#2310=ADVANCED_FACE('',(#281),#66,.F.);
#2311=ADVANCED_FACE('',(#282),#2223,.F.);
#2312=ADVANCED_FACE('',(#283),#2224,.T.);
#2313=ADVANCED_FACE('',(#284),#2225,.T.);
#2314=ADVANCED_FACE('',(#285),#67,.F.);
#2315=ADVANCED_FACE('',(#286),#2226,.F.);
#2316=ADVANCED_FACE('',(#287),#2227,.T.);
#2317=ADVANCED_FACE('',(#288),#2228,.T.);
#2318=ADVANCED_FACE('',(#289),#68,.F.);
#2319=ADVANCED_FACE('',(#290),#2229,.F.);
#2320=ADVANCED_FACE('',(#291),#2230,.T.);
#2321=ADVANCED_FACE('',(#292),#2231,.T.);
#2322=ADVANCED_FACE('',(#293),#69,.F.);
#2323=ADVANCED_FACE('',(#294),#2232,.F.);
#2324=ADVANCED_FACE('',(#295),#2233,.T.);
#2325=ADVANCED_FACE('',(#296),#2234,.T.);
#2326=ADVANCED_FACE('',(#297),#70,.F.);
#2327=ADVANCED_FACE('',(#298),#2235,.F.);
#2328=ADVANCED_FACE('',(#299),#2236,.T.);
#2329=ADVANCED_FACE('',(#300),#2237,.T.);
#2330=ADVANCED_FACE('',(#301),#71,.F.);
#2331=ADVANCED_FACE('',(#302),#2238,.F.);
#2332=ADVANCED_FACE('',(#303),#2239,.T.);
#2333=ADVANCED_FACE('',(#304),#2240,.T.);
#2334=ADVANCED_FACE('',(#305),#2241,.T.);
#2335=ADVANCED_FACE('',(#306),#72,.F.);
#2336=ADVANCED_FACE('',(#307),#2242,.F.);
#2337=ADVANCED_FACE('',(#308),#2243,.T.);
#2338=ADVANCED_FACE('',(#309,#49),#73,.T.);
#2339=ADVANCED_FACE('',(#310,#50),#74,.T.);
#2340=ADVANCED_FACE('',(#311),#39,.T.);
#2341=ADVANCED_FACE('',(#312,#51),#2244,.T.);
#2342=ADVANCED_FACE('',(#313),#40,.T.);
#2343=ADVANCED_FACE('',(#314,#52),#75,.T.);
#2344=ADVANCED_FACE('',(#315),#41,.F.);
#2345=ADVANCED_FACE('',(#316),#42,.T.);
#2346=ADVANCED_FACE('',(#317,#53),#76,.T.);
#2347=ADVANCED_FACE('',(#318),#43,.F.);
#2348=ADVANCED_FACE('',(#319),#44,.F.);
#2349=ADVANCED_FACE('',(#320,#54),#77,.T.);
#2350=ADVANCED_FACE('',(#321),#45,.T.);
#2351=ADVANCED_FACE('',(#322),#46,.F.);
#2352=ADVANCED_FACE('',(#323,#55),#78,.T.);
#2353=ADVANCED_FACE('',(#324),#47,.T.);
#2354=ADVANCED_FACE('',(#325),#2245,.T.);
#2355=ADVANCED_FACE('',(#326),#48,.T.);
#2356=ADVANCED_FACE('',(#327),#2246,.T.);
#2357=ADVANCED_FACE('',(#328),#2247,.T.);
#2358=ADVANCED_FACE('',(#329),#2248,.T.);
#2359=ADVANCED_FACE('',(#330),#2249,.T.);
#2360=ADVANCED_FACE('',(#331),#2250,.T.);
#2361=ADVANCED_FACE('',(#332),#2251,.T.);
#2362=ADVANCED_FACE('',(#333),#2252,.T.);
#2363=ADVANCED_FACE('',(#334),#2253,.T.);
#2364=ADVANCED_FACE('',(#335),#2254,.T.);
#2365=ADVANCED_FACE('',(#336),#2255,.T.);
#2366=ADVANCED_FACE('',(#337),#2256,.T.);
#2367=ADVANCED_FACE('',(#338),#2257,.T.);
#2368=ADVANCED_FACE('',(#339),#2258,.T.);
#2369=ADVANCED_FACE('',(#340),#2259,.T.);
#2370=ADVANCED_FACE('',(#341),#23,.F.);
#2371=ADVANCED_FACE('',(#342),#24,.F.);
#2372=ADVANCED_FACE('',(#343,#56),#79,.T.);
#2373=ADVANCED_FACE('',(#344),#80,.F.);
#2374=ADVANCED_FACE('',(#345),#81,.F.);
#2375=ADVANCED_FACE('',(#346),#82,.F.);
#2376=ADVANCED_FACE('',(#347),#83,.F.);
#2377=ADVANCED_FACE('',(#348),#84,.F.);
#2378=ADVANCED_FACE('',(#349),#85,.F.);
#2379=ADVANCED_FACE('',(#350),#86,.F.);
#2380=ADVANCED_FACE('',(#351),#87,.F.);
#2381=ADVANCED_FACE('',(#352),#2260,.T.);
#2382=ADVANCED_FACE('',(#353),#2261,.T.);
#2383=ADVANCED_FACE('',(#354),#2262,.T.);
#2384=ADVANCED_FACE('',(#355),#2263,.T.);
#2385=ADVANCED_FACE('',(#356),#2264,.T.);
#2386=ADVANCED_FACE('',(#357),#2265,.T.);
#2387=ADVANCED_FACE('',(#358),#2266,.T.);
#2388=ADVANCED_FACE('',(#359),#2267,.T.);
#2389=ADVANCED_FACE('',(#360),#2268,.T.);
#2390=ADVANCED_FACE('',(#361),#2269,.T.);
#2391=ADVANCED_FACE('',(#362),#2270,.T.);
#2392=ADVANCED_FACE('',(#363),#2271,.T.);
#2393=ADVANCED_FACE('',(#364),#2272,.T.);
#2394=ADVANCED_FACE('',(#365),#2273,.T.);
#2395=ADVANCED_FACE('',(#366),#25,.F.);
#2396=ADVANCED_FACE('',(#367),#26,.F.);
#2397=ADVANCED_FACE('',(#368,#57),#88,.T.);
#2398=ADVANCED_FACE('',(#369),#89,.F.);
#2399=ADVANCED_FACE('',(#370),#90,.F.);
#2400=ADVANCED_FACE('',(#371),#91,.F.);
#2401=ADVANCED_FACE('',(#372),#92,.F.);
#2402=ADVANCED_FACE('',(#373),#93,.F.);
#2403=ADVANCED_FACE('',(#374),#94,.F.);
#2404=ADVANCED_FACE('',(#375),#95,.F.);
#2405=ADVANCED_FACE('',(#376),#96,.F.);
#2406=CLOSED_SHELL('',(#2274,#2275,#2276,#2277,#2278,#2279,#2280,#2281,
#2282,#2283,#2284,#2285,#2286,#2287,#2288,#2289,#2290,#2291,#2292,#2293,
#2294,#2295,#2296,#2297,#2298,#2299,#2300,#2301,#2302,#2303,#2304,#2305,
#2306,#2307,#2308,#2309,#2310,#2311,#2312,#2313,#2314,#2315,#2316,#2317,
#2318,#2319,#2320,#2321,#2322,#2323,#2324,#2325,#2326,#2327,#2328,#2329,
#2330,#2331,#2332,#2333,#2334,#2335,#2336,#2337,#2338,#2339,#2340,#2341,
#2342,#2343,#2344,#2345,#2346,#2347,#2348,#2349,#2350,#2351,#2352,#2353,
#2354,#2355));
#2407=CLOSED_SHELL('',(#2356,#2357,#2358,#2359,#2360,#2361,#2362,#2363,
#2364,#2365,#2366,#2367,#2368,#2369,#2370,#2371,#2372,#2373,#2374,#2375,
#2376,#2377,#2378,#2379,#2380));
#2408=CLOSED_SHELL('',(#2381,#2382,#2383,#2384,#2385,#2386,#2387,#2388,
#2389,#2390,#2391,#2392,#2393,#2394,#2395,#2396,#2397,#2398,#2399,#2400,
#2401,#2402,#2403,#2404,#2405));
#2409=DERIVED_UNIT_ELEMENT(#2415,1.);
#2410=DERIVED_UNIT_ELEMENT(#12120,-3.);
#2411=DERIVED_UNIT_ELEMENT(#2415,1.);
#2412=DERIVED_UNIT_ELEMENT(#12120,-3.);
#2413=DERIVED_UNIT_ELEMENT(#2415,1.);
#2414=DERIVED_UNIT_ELEMENT(#12120,-3.);
#2415=(
MASS_UNIT()
NAMED_UNIT(*)
SI_UNIT(.KILO.,.GRAM.)
);
#2416=DERIVED_UNIT((#2409,#2410));
#2417=DERIVED_UNIT((#2411,#2412));
#2418=DERIVED_UNIT((#2413,#2414));
#2419=MEASURE_REPRESENTATION_ITEM('density measure',
POSITIVE_RATIO_MEASURE(7850.),#2416);
#2420=MEASURE_REPRESENTATION_ITEM('density measure',
POSITIVE_RATIO_MEASURE(7850.),#2417);
#2421=MEASURE_REPRESENTATION_ITEM('density measure',
POSITIVE_RATIO_MEASURE(7850.),#2418);
#2422=PROPERTY_DEFINITION_REPRESENTATION(#2437,#2428);
#2423=PROPERTY_DEFINITION_REPRESENTATION(#2438,#2429);
#2424=PROPERTY_DEFINITION_REPRESENTATION(#2439,#2430);
#2425=PROPERTY_DEFINITION_REPRESENTATION(#2440,#2431);
#2426=PROPERTY_DEFINITION_REPRESENTATION(#2441,#2432);
#2427=PROPERTY_DEFINITION_REPRESENTATION(#2442,#2433);
#2428=REPRESENTATION('material name',(#2434),#12115);
#2429=REPRESENTATION('density',(#2419),#12115);
#2430=REPRESENTATION('material name',(#2435),#12116);
#2431=REPRESENTATION('density',(#2420),#12116);
#2432=REPRESENTATION('material name',(#2436),#12117);
#2433=REPRESENTATION('density',(#2421),#12117);
#2434=DESCRIPTIVE_REPRESENTATION_ITEM('Steel','Steel');
#2435=DESCRIPTIVE_REPRESENTATION_ITEM('Steel','Steel');
#2436=DESCRIPTIVE_REPRESENTATION_ITEM('Steel','Steel');
#2437=PROPERTY_DEFINITION('material property','material name',#12140);
#2438=PROPERTY_DEFINITION('material property','density of part',#12140);
#2439=PROPERTY_DEFINITION('material property','material name',#12141);
#2440=PROPERTY_DEFINITION('material property','density of part',#12141);
#2441=PROPERTY_DEFINITION('material property','material name',#12142);
#2442=PROPERTY_DEFINITION('material property','density of part',#12142);
#2443=AXIS2_PLACEMENT_3D('',#3430,#2726,#2727);
#2444=AXIS2_PLACEMENT_3D('',#3431,#2728,#2729);
#2445=AXIS2_PLACEMENT_3D('',#3432,#2730,#2731);
#2446=AXIS2_PLACEMENT_3D('',#3525,#2733,#2734);
#2447=AXIS2_PLACEMENT_3D('',#3527,#2735,#2736);
#2448=AXIS2_PLACEMENT_3D('',#3558,#2739,#2740);
#2449=AXIS2_PLACEMENT_3D('',#3575,#2741,#2742);
#2450=AXIS2_PLACEMENT_3D('',#3618,#2744,#2745);
#2451=AXIS2_PLACEMENT_3D('',#3623,#2747,#2748);
#2452=AXIS2_PLACEMENT_3D('',#3626,#2750,#2751);
#2453=AXIS2_PLACEMENT_3D('',#3627,#2752,#2753);
#2454=AXIS2_PLACEMENT_3D('',#3629,#2754,#2755);
#2455=AXIS2_PLACEMENT_3D('',#3631,#2756,#2757);
#2456=AXIS2_PLACEMENT_3D('',#3632,#2758,#2759);
#2457=AXIS2_PLACEMENT_3D('',#3633,#2760,#2761);
#2458=AXIS2_PLACEMENT_3D('',#3635,#2762,#2763);
#2459=AXIS2_PLACEMENT_3D('',#3637,#2765,#2766);
#2460=AXIS2_PLACEMENT_3D('',#3640,#2768,#2769);
#2461=AXIS2_PLACEMENT_3D('',#3641,#2770,#2771);
#2462=AXIS2_PLACEMENT_3D('',#3646,#2773,#2774);
#2463=AXIS2_PLACEMENT_3D('',#3649,#2776,#2777);
#2464=AXIS2_PLACEMENT_3D('',#3650,#2778,#2779);
#2465=AXIS2_PLACEMENT_3D('',#3652,#2780,#2781);
#2466=AXIS2_PLACEMENT_3D('',#3654,#2782,#2783);
#2467=AXIS2_PLACEMENT_3D('',#3655,#2784,#2785);
#2468=AXIS2_PLACEMENT_3D('',#3656,#2786,#2787);
#2469=AXIS2_PLACEMENT_3D('',#3658,#2788,#2789);
#2470=AXIS2_PLACEMENT_3D('',#3660,#2791,#2792);
#2471=AXIS2_PLACEMENT_3D('',#3663,#2794,#2795);
#2472=AXIS2_PLACEMENT_3D('',#3664,#2796,#2797);
#2473=AXIS2_PLACEMENT_3D('',#3669,#2799,#2800);
#2474=AXIS2_PLACEMENT_3D('',#3672,#2802,#2803);
#2475=AXIS2_PLACEMENT_3D('',#3673,#2804,#2805);
#2476=AXIS2_PLACEMENT_3D('',#3675,#2806,#2807);
#2477=AXIS2_PLACEMENT_3D('',#3677,#2808,#2809);
#2478=AXIS2_PLACEMENT_3D('',#3678,#2810,#2811);
#2479=AXIS2_PLACEMENT_3D('',#3679,#2812,#2813);
#2480=AXIS2_PLACEMENT_3D('',#3681,#2814,#2815);
#2481=AXIS2_PLACEMENT_3D('',#3683,#2817,#2818);
#2482=AXIS2_PLACEMENT_3D('',#3686,#2820,#2821);
#2483=AXIS2_PLACEMENT_3D('',#3687,#2822,#2823);
#2484=AXIS2_PLACEMENT_3D('',#3692,#2825,#2826);
#2485=AXIS2_PLACEMENT_3D('',#3695,#2828,#2829);
#2486=AXIS2_PLACEMENT_3D('',#3696,#2830,#2831);
#2487=AXIS2_PLACEMENT_3D('',#3698,#2832,#2833);
#2488=AXIS2_PLACEMENT_3D('',#3700,#2834,#2835);
#2489=AXIS2_PLACEMENT_3D('',#3701,#2836,#2837);
#2490=AXIS2_PLACEMENT_3D('',#3702,#2838,#2839);
#2491=AXIS2_PLACEMENT_3D('',#3704,#2840,#2841);
#2492=AXIS2_PLACEMENT_3D('',#3706,#2843,#2844);
#2493=AXIS2_PLACEMENT_3D('',#3709,#2846,#2847);
#2494=AXIS2_PLACEMENT_3D('',#3710,#2848,#2849);
#2495=AXIS2_PLACEMENT_3D('',#3715,#2851,#2852);
#2496=AXIS2_PLACEMENT_3D('',#3718,#2854,#2855);
#2497=AXIS2_PLACEMENT_3D('',#3719,#2856,#2857);
#2498=AXIS2_PLACEMENT_3D('',#3721,#2858,#2859);
#2499=AXIS2_PLACEMENT_3D('',#3723,#2860,#2861);
#2500=AXIS2_PLACEMENT_3D('',#3724,#2862,#2863);
#2501=AXIS2_PLACEMENT_3D('',#3725,#2864,#2865);
#2502=AXIS2_PLACEMENT_3D('',#3727,#2866,#2867);
#2503=AXIS2_PLACEMENT_3D('',#3729,#2869,#2870);
#2504=AXIS2_PLACEMENT_3D('',#3732,#2872,#2873);
#2505=AXIS2_PLACEMENT_3D('',#3733,#2874,#2875);
#2506=AXIS2_PLACEMENT_3D('',#3738,#2877,#2878);
#2507=AXIS2_PLACEMENT_3D('',#3741,#2880,#2881);
#2508=AXIS2_PLACEMENT_3D('',#3742,#2882,#2883);
#2509=AXIS2_PLACEMENT_3D('',#3744,#2884,#2885);
#2510=AXIS2_PLACEMENT_3D('',#3746,#2886,#2887);
#2511=AXIS2_PLACEMENT_3D('',#3747,#2888,#2889);
#2512=AXIS2_PLACEMENT_3D('',#3748,#2890,#2891);
#2513=AXIS2_PLACEMENT_3D('',#3750,#2892,#2893);
#2514=AXIS2_PLACEMENT_3D('',#3752,#2895,#2896);
#2515=AXIS2_PLACEMENT_3D('',#3755,#2898,#2899);
#2516=AXIS2_PLACEMENT_3D('',#3756,#2900,#2901);
#2517=AXIS2_PLACEMENT_3D('',#3761,#2903,#2904);
#2518=AXIS2_PLACEMENT_3D('',#3764,#2906,#2907);
#2519=AXIS2_PLACEMENT_3D('',#3765,#2908,#2909);
#2520=AXIS2_PLACEMENT_3D('',#3767,#2910,#2911);
#2521=AXIS2_PLACEMENT_3D('',#3769,#2912,#2913);
#2522=AXIS2_PLACEMENT_3D('',#3770,#2914,#2915);
#2523=AXIS2_PLACEMENT_3D('',#3771,#2916,#2917);
#2524=AXIS2_PLACEMENT_3D('',#3773,#2918,#2919);
#2525=AXIS2_PLACEMENT_3D('',#3775,#2921,#2922);
#2526=AXIS2_PLACEMENT_3D('',#3778,#2924,#2925);
#2527=AXIS2_PLACEMENT_3D('',#3779,#2926,#2927);
#2528=AXIS2_PLACEMENT_3D('',#3784,#2929,#2930);
#2529=AXIS2_PLACEMENT_3D('',#3787,#2932,#2933);
#2530=AXIS2_PLACEMENT_3D('',#3788,#2934,#2935);
#2531=AXIS2_PLACEMENT_3D('',#3790,#2936,#2937);
#2532=AXIS2_PLACEMENT_3D('',#3792,#2938,#2939);
#2533=AXIS2_PLACEMENT_3D('',#3793,#2940,#2941);
#2534=AXIS2_PLACEMENT_3D('',#3794,#2942,#2943);
#2535=AXIS2_PLACEMENT_3D('',#3796,#2944,#2945);
#2536=AXIS2_PLACEMENT_3D('',#3798,#2947,#2948);
#2537=AXIS2_PLACEMENT_3D('',#3801,#2950,#2951);
#2538=AXIS2_PLACEMENT_3D('',#3802,#2952,#2953);
#2539=AXIS2_PLACEMENT_3D('',#3807,#2955,#2956);
#2540=AXIS2_PLACEMENT_3D('',#3810,#2958,#2959);
#2541=AXIS2_PLACEMENT_3D('',#3811,#2960,#2961);
#2542=AXIS2_PLACEMENT_3D('',#3813,#2962,#2963);
#2543=AXIS2_PLACEMENT_3D('',#3815,#2964,#2965);
#2544=AXIS2_PLACEMENT_3D('',#3816,#2966,#2967);
#2545=AXIS2_PLACEMENT_3D('',#3817,#2968,#2969);
#2546=AXIS2_PLACEMENT_3D('',#3819,#2970,#2971);
#2547=AXIS2_PLACEMENT_3D('',#3821,#2973,#2974);
#2548=AXIS2_PLACEMENT_3D('',#3824,#2976,#2977);
#2549=AXIS2_PLACEMENT_3D('',#3825,#2978,#2979);
#2550=AXIS2_PLACEMENT_3D('',#3830,#2981,#2982);
#2551=AXIS2_PLACEMENT_3D('',#3833,#2984,#2985);
#2552=AXIS2_PLACEMENT_3D('',#3834,#2986,#2987);
#2553=AXIS2_PLACEMENT_3D('',#3836,#2988,#2989);
#2554=AXIS2_PLACEMENT_3D('',#3838,#2990,#2991);
#2555=AXIS2_PLACEMENT_3D('',#3839,#2992,#2993);
#2556=AXIS2_PLACEMENT_3D('',#3840,#2994,#2995);
#2557=AXIS2_PLACEMENT_3D('',#3842,#2996,#2997);
#2558=AXIS2_PLACEMENT_3D('',#3844,#2999,#3000);
#2559=AXIS2_PLACEMENT_3D('',#3847,#3002,#3003);
#2560=AXIS2_PLACEMENT_3D('',#3848,#3004,#3005);
#2561=AXIS2_PLACEMENT_3D('',#3853,#3007,#3008);
#2562=AXIS2_PLACEMENT_3D('',#3856,#3010,#3011);
#2563=AXIS2_PLACEMENT_3D('',#3857,#3012,#3013);
#2564=AXIS2_PLACEMENT_3D('',#3859,#3014,#3015);
#2565=AXIS2_PLACEMENT_3D('',#3861,#3016,#3017);
#2566=AXIS2_PLACEMENT_3D('',#3862,#3018,#3019);
#2567=AXIS2_PLACEMENT_3D('',#3863,#3020,#3021);
#2568=AXIS2_PLACEMENT_3D('',#3865,#3022,#3023);
#2569=AXIS2_PLACEMENT_3D('',#3867,#3025,#3026);
#2570=AXIS2_PLACEMENT_3D('',#3870,#3028,#3029);
#2571=AXIS2_PLACEMENT_3D('',#3871,#3030,#3031);
#2572=AXIS2_PLACEMENT_3D('',#3876,#3033,#3034);
#2573=AXIS2_PLACEMENT_3D('',#3879,#3036,#3037);
#2574=AXIS2_PLACEMENT_3D('',#3880,#3038,#3039);
#2575=AXIS2_PLACEMENT_3D('',#3882,#3040,#3041);
#2576=AXIS2_PLACEMENT_3D('',#3884,#3042,#3043);
#2577=AXIS2_PLACEMENT_3D('',#3885,#3044,#3045);
#2578=AXIS2_PLACEMENT_3D('',#3886,#3046,#3047);
#2579=AXIS2_PLACEMENT_3D('',#3888,#3048,#3049);
#2580=AXIS2_PLACEMENT_3D('',#3890,#3051,#3052);
#2581=AXIS2_PLACEMENT_3D('',#3893,#3054,#3055);
#2582=AXIS2_PLACEMENT_3D('',#3894,#3056,#3057);
#2583=AXIS2_PLACEMENT_3D('',#3899,#3059,#3060);
#2584=AXIS2_PLACEMENT_3D('',#3902,#3062,#3063);
#2585=AXIS2_PLACEMENT_3D('',#3903,#3064,#3065);
#2586=AXIS2_PLACEMENT_3D('',#3905,#3066,#3067);
#2587=AXIS2_PLACEMENT_3D('',#3907,#3068,#3069);
#2588=AXIS2_PLACEMENT_3D('',#3908,#3070,#3071);
#2589=AXIS2_PLACEMENT_3D('',#3909,#3072,#3073);
#2590=AXIS2_PLACEMENT_3D('',#3911,#3074,#3075);
#2591=AXIS2_PLACEMENT_3D('',#3913,#3077,#3078);
#2592=AXIS2_PLACEMENT_3D('',#3916,#3080,#3081);
#2593=AXIS2_PLACEMENT_3D('',#3917,#3082,#3083);
#2594=AXIS2_PLACEMENT_3D('',#3922,#3085,#3086);
#2595=AXIS2_PLACEMENT_3D('',#3925,#3088,#3089);
#2596=AXIS2_PLACEMENT_3D('',#3926,#3090,#3091);
#2597=AXIS2_PLACEMENT_3D('',#3928,#3092,#3093);
#2598=AXIS2_PLACEMENT_3D('',#3930,#3094,#3095);
#2599=AXIS2_PLACEMENT_3D('',#3931,#3096,#3097);
#2600=AXIS2_PLACEMENT_3D('',#3932,#3098,#3099);
#2601=AXIS2_PLACEMENT_3D('',#3934,#3100,#3101);
#2602=AXIS2_PLACEMENT_3D('',#3936,#3103,#3104);
#2603=AXIS2_PLACEMENT_3D('',#3939,#3106,#3107);
#2604=AXIS2_PLACEMENT_3D('',#3940,#3108,#3109);
#2605=AXIS2_PLACEMENT_3D('',#3943,#3110,#3111);
#2606=AXIS2_PLACEMENT_3D('',#3946,#3113,#3114);
#2607=AXIS2_PLACEMENT_3D('',#3948,#3115,#3116);
#2608=AXIS2_PLACEMENT_3D('',#3951,#3118,#3119);
#2609=AXIS2_PLACEMENT_3D('',#3952,#3120,#3121);
#2610=AXIS2_PLACEMENT_3D('',#3953,#3122,#3123);
#2611=AXIS2_PLACEMENT_3D('',#3954,#3124,#3125);
#2612=AXIS2_PLACEMENT_3D('',#3955,#3126,#3127);
#2613=AXIS2_PLACEMENT_3D('',#3956,#3128,#3129);
#2614=AXIS2_PLACEMENT_3D('',#3957,#3130,#3131);
#2615=AXIS2_PLACEMENT_3D('',#3958,#3132,#3133);
#2616=AXIS2_PLACEMENT_3D('',#3959,#3134,#3135);
#2617=AXIS2_PLACEMENT_3D('',#3960,#3136,#3137);
#2618=AXIS2_PLACEMENT_3D('',#3961,#3138,#3139);
#2619=AXIS2_PLACEMENT_3D('',#3962,#3140,#3141);
#2620=AXIS2_PLACEMENT_3D('',#3963,#3142,#3143);
#2621=AXIS2_PLACEMENT_3D('',#3964,#3144,#3145);
#2622=AXIS2_PLACEMENT_3D('',#3966,#3146,#3147);
#2623=AXIS2_PLACEMENT_3D('',#3968,#3149,#3150);
#2624=AXIS2_PLACEMENT_3D('',#3970,#3151,#3152);
#2625=AXIS2_PLACEMENT_3D('',#3973,#3154,#3155);
#2626=AXIS2_PLACEMENT_3D('',#3974,#3156,#3157);
#2627=AXIS2_PLACEMENT_3D('',#3976,#3158,#3159);
#2628=AXIS2_PLACEMENT_3D('',#3977,#3160,#3161);
#2629=AXIS2_PLACEMENT_3D('',#3978,#3162,#3163);
#2630=AXIS2_PLACEMENT_3D('',#3980,#3164,#3165);
#2631=AXIS2_PLACEMENT_3D('',#3982,#3167,#3168);
#2632=AXIS2_PLACEMENT_3D('',#3983,#3169,#3170);
#2633=AXIS2_PLACEMENT_3D('',#3984,#3171,#3172);
#2634=AXIS2_PLACEMENT_3D('',#3986,#3173,#3174);
#2635=AXIS2_PLACEMENT_3D('',#3987,#3175,#3176);
#2636=AXIS2_PLACEMENT_3D('',#3989,#3177,#3178);
#2637=AXIS2_PLACEMENT_3D('',#3990,#3179,#3180);
#2638=AXIS2_PLACEMENT_3D('',#3992,#3181,#3182);
#2639=AXIS2_PLACEMENT_3D('',#3994,#3184,#3185);
#2640=AXIS2_PLACEMENT_3D('',#3996,#3186,#3187);
#2641=AXIS2_PLACEMENT_3D('',#3999,#3190,#3191);
#2642=AXIS2_PLACEMENT_3D('',#4002,#3193,#3194);
#2643=AXIS2_PLACEMENT_3D('',#4003,#3195,#3196);
#2644=AXIS2_PLACEMENT_3D('',#4005,#3197,#3198);
#2645=AXIS2_PLACEMENT_3D('',#4006,#3199,#3200);
#2646=AXIS2_PLACEMENT_3D('',#4008,#3201,#3202);
#2647=AXIS2_PLACEMENT_3D('',#4010,#3204,#3205);
#2648=AXIS2_PLACEMENT_3D('',#4013,#3207,#3208);
#2649=AXIS2_PLACEMENT_3D('',#4014,#3209,#3210);
#2650=AXIS2_PLACEMENT_3D('',#4016,#3211,#3212);
#2651=AXIS2_PLACEMENT_3D('',#4017,#3213,#3214);
#2652=AXIS2_PLACEMENT_3D('',#4019,#3216,#3217);
#2653=AXIS2_PLACEMENT_3D('',#4022,#3219,#3220);
#2654=AXIS2_PLACEMENT_3D('',#4023,#3221,#3222);
#2655=AXIS2_PLACEMENT_3D('',#4025,#3223,#3224);
#2656=AXIS2_PLACEMENT_3D('',#4026,#3225,#3226);
#2657=AXIS2_PLACEMENT_3D('',#4028,#3227,#3228);
#2658=AXIS2_PLACEMENT_3D('',#4030,#3230,#3231);
#2659=AXIS2_PLACEMENT_3D('',#4033,#3233,#3234);
#2660=AXIS2_PLACEMENT_3D('',#4034,#3235,#3236);
#2661=AXIS2_PLACEMENT_3D('',#4036,#3237,#3238);
#2662=AXIS2_PLACEMENT_3D('',#4037,#3239,#3240);
#2663=AXIS2_PLACEMENT_3D('',#4039,#3241,#3242);
#2664=AXIS2_PLACEMENT_3D('',#4041,#3244,#3245);
#2665=AXIS2_PLACEMENT_3D('',#4043,#3246,#3247);
#2666=AXIS2_PLACEMENT_3D('',#4045,#3249,#3250);
#2667=AXIS2_PLACEMENT_3D('',#4047,#3252,#3253);
#2668=AXIS2_PLACEMENT_3D('',#4048,#3254,#3255);
#2669=AXIS2_PLACEMENT_3D('',#4202,#3257,#3258);
#2670=AXIS2_PLACEMENT_3D('',#4315,#3259,#3260);
#2671=AXIS2_PLACEMENT_3D('',#4339,#3262,#3263);
#2672=AXIS2_PLACEMENT_3D('',#4651,#3265,#3266);
#2673=AXIS2_PLACEMENT_3D('',#4969,#3268,#3269);
#2674=AXIS2_PLACEMENT_3D('',#5317,#3271,#3272);
#2675=AXIS2_PLACEMENT_3D('',#5503,#3274,#3275);
#2676=AXIS2_PLACEMENT_3D('',#5570,#3277,#3278);
#2677=AXIS2_PLACEMENT_3D('',#5605,#3279,#3280);
#2678=AXIS2_PLACEMENT_3D('',#5989,#3282,#3283);
#2679=AXIS2_PLACEMENT_3D('',#6373,#3285,#3286);
#2680=AXIS2_PLACEMENT_3D('',#6578,#3288,#3289);
#2681=AXIS2_PLACEMENT_3D('',#6782,#3291,#3292);
#2682=AXIS2_PLACEMENT_3D('',#7166,#3294,#3295);
#2683=AXIS2_PLACEMENT_3D('',#7296,#3296,#3297);
#2684=AXIS2_PLACEMENT_3D('',#7304,#3298,#3299);
#2685=AXIS2_PLACEMENT_3D('',#7344,#3300,#3301);
#2686=AXIS2_PLACEMENT_3D('',#8036,#3302,#3303);
#2687=AXIS2_PLACEMENT_3D('',#8049,#3310,#3311);
#2688=AXIS2_PLACEMENT_3D('',#8055,#3315,#3316);
#2689=AXIS2_PLACEMENT_3D('',#8059,#3319,#3320);
#2690=AXIS2_PLACEMENT_3D('',#8063,#3323,#3324);
#2691=AXIS2_PLACEMENT_3D('',#8067,#3327,#3328);
#2692=AXIS2_PLACEMENT_3D('',#8071,#3331,#3332);
#2693=AXIS2_PLACEMENT_3D('',#8073,#3334,#3335);
#2694=AXIS2_PLACEMENT_3D('',#8074,#3336,#3337);
#2695=AXIS2_PLACEMENT_3D('',#8075,#3338,#3339);
#2696=AXIS2_PLACEMENT_3D('',#8076,#3340,#3341);
#2697=AXIS2_PLACEMENT_3D('',#8230,#3343,#3344);
#2698=AXIS2_PLACEMENT_3D('',#8343,#3345,#3346);
#2699=AXIS2_PLACEMENT_3D('',#8367,#3348,#3349);
#2700=AXIS2_PLACEMENT_3D('',#8681,#3351,#3352);
#2701=AXIS2_PLACEMENT_3D('',#8997,#3354,#3355);
#2702=AXIS2_PLACEMENT_3D('',#9345,#3357,#3358);
#2703=AXIS2_PLACEMENT_3D('',#9531,#3360,#3361);
#2704=AXIS2_PLACEMENT_3D('',#9598,#3363,#3364);
#2705=AXIS2_PLACEMENT_3D('',#9633,#3365,#3366);
#2706=AXIS2_PLACEMENT_3D('',#10017,#3368,#3369);
#2707=AXIS2_PLACEMENT_3D('',#10401,#3371,#3372);
#2708=AXIS2_PLACEMENT_3D('',#10606,#3374,#3375);
#2709=AXIS2_PLACEMENT_3D('',#10810,#3377,#3378);
#2710=AXIS2_PLACEMENT_3D('',#11194,#3380,#3381);
#2711=AXIS2_PLACEMENT_3D('',#11324,#3382,#3383);
#2712=AXIS2_PLACEMENT_3D('',#11332,#3384,#3385);
#2713=AXIS2_PLACEMENT_3D('',#11372,#3386,#3387);
#2714=AXIS2_PLACEMENT_3D('',#12067,#3388,#3389);
#2715=AXIS2_PLACEMENT_3D('',#12080,#3396,#3397);
#2716=AXIS2_PLACEMENT_3D('',#12086,#3401,#3402);
#2717=AXIS2_PLACEMENT_3D('',#12090,#3405,#3406);
#2718=AXIS2_PLACEMENT_3D('',#12094,#3409,#3410);
#2719=AXIS2_PLACEMENT_3D('',#12098,#3413,#3414);
#2720=AXIS2_PLACEMENT_3D('',#12102,#3417,#3418);
#2721=AXIS2_PLACEMENT_3D('',#12104,#3420,#3421);
#2722=AXIS2_PLACEMENT_3D('',#12105,#3422,#3423);
#2723=AXIS2_PLACEMENT_3D('',#12106,#3424,#3425);
#2724=AXIS2_PLACEMENT_3D('',#12107,#3426,#3427);
#2725=AXIS2_PLACEMENT_3D('',#12108,#3428,#3429);
#2726=DIRECTION('axis',(0.,0.,1.));
#2727=DIRECTION('refdir',(1.,0.,0.));
#2728=DIRECTION('axis',(0.,0.,1.));
#2729=DIRECTION('refdir',(1.,0.,0.));
#2730=DIRECTION('center_axis',(0.,1.,0.));
#2731=DIRECTION('ref_axis',(1.,0.,0.));
#2732=DIRECTION('',(0.,1.,0.));
#2733=DIRECTION('center_axis',(0.,0.,-1.));
#2734=DIRECTION('ref_axis',(-1.,0.,0.));
#2735=DIRECTION('center_axis',(0.,0.,-1.));
#2736=DIRECTION('ref_axis',(1.,0.,0.));
#2737=DIRECTION('',(0.,0.,-1.));
#2738=DIRECTION('',(0.,0.,-1.));
#2739=DIRECTION('center_axis',(0.,0.,-1.));
#2740=DIRECTION('ref_axis',(1.,0.,0.));
#2741=DIRECTION('center_axis',(1.,0.,0.));
#2742=DIRECTION('ref_axis',(0.,1.,0.));
#2743=DIRECTION('',(1.,0.,0.));
#2744=DIRECTION('center_axis',(0.,0.,1.));
#2745=DIRECTION('ref_axis',(0.975941703326222,0.218031630064795,0.));
#2746=DIRECTION('',(0.,0.,1.));
#2747=DIRECTION('center_axis',(0.,0.,1.));
#2748=DIRECTION('ref_axis',(0.975941703326222,0.218031630064795,0.));
#2749=DIRECTION('',(0.,0.,1.));
#2750=DIRECTION('center_axis',(0.,0.,-1.));
#2751=DIRECTION('ref_axis',(0.975941703326222,0.218031630064795,0.));
#2752=DIRECTION('center_axis',(0.,0.,1.));
#2753=DIRECTION('ref_axis',(-0.913545457642601,-0.406736643075801,0.));
#2754=DIRECTION('center_axis',(0.,0.,1.));
#2755=DIRECTION('ref_axis',(-1.,0.,0.));
#2756=DIRECTION('center_axis',(0.,0.,1.));
#2757=DIRECTION('ref_axis',(-0.611669535952668,0.791113379224146,0.));
#2758=DIRECTION('center_axis',(0.,0.,-1.));
#2759=DIRECTION('ref_axis',(0.591883195117478,-0.806023748618815,0.));
#2760=DIRECTION('center_axis',(0.,0.,1.));
#2761=DIRECTION('ref_axis',(-0.611669535952668,0.791113379224146,0.));
#2762=DIRECTION('center_axis',(0.,0.,1.));
#2763=DIRECTION('ref_axis',(-0.611669535952668,0.791113379224146,0.));
#2764=DIRECTION('',(0.,0.,1.));
#2765=DIRECTION('center_axis',(0.,0.,1.));
#2766=DIRECTION('ref_axis',(0.591883195117478,-0.806023748618815,0.));
#2767=DIRECTION('',(0.,0.,-1.));
#2768=DIRECTION('center_axis',(0.,0.,1.));
#2769=DIRECTION('ref_axis',(0.591883195117478,-0.806023748618815,0.));
#2770=DIRECTION('center_axis',(0.,0.,1.));
#2771=DIRECTION('ref_axis',(0.802885656700754,0.596133057516692,0.));
#2772=DIRECTION('',(0.,0.,1.));
#2773=DIRECTION('center_axis',(0.,0.,1.));
#2774=DIRECTION('ref_axis',(0.802885656700754,0.596133057516692,0.));
#2775=DIRECTION('',(0.,0.,1.));
#2776=DIRECTION('center_axis',(0.,0.,-1.));
#2777=DIRECTION('ref_axis',(0.802885656700754,0.596133057516692,0.));
#2778=DIRECTION('center_axis',(0.,0.,1.));
#2779=DIRECTION('ref_axis',(-0.669130606358858,-0.743144825477395,0.));
#2780=DIRECTION('center_axis',(0.,0.,1.));
#2781=DIRECTION('ref_axis',(-1.,0.,0.));
#2782=DIRECTION('center_axis',(0.,0.,1.));
#2783=DIRECTION('ref_axis',(-0.880562726305899,0.473929620345386,0.));
#2784=DIRECTION('center_axis',(0.,0.,-1.));
#2785=DIRECTION('ref_axis',(0.86855159810715,-0.495598750427718,0.));
#2786=DIRECTION('center_axis',(0.,0.,1.));
#2787=DIRECTION('ref_axis',(-0.880562726305899,0.473929620345386,0.));
#2788=DIRECTION('center_axis',(0.,0.,1.));
#2789=DIRECTION('ref_axis',(-0.880562726305899,0.473929620345386,0.));
#2790=DIRECTION('',(0.,0.,1.));
#2791=DIRECTION('center_axis',(0.,0.,1.));
#2792=DIRECTION('ref_axis',(0.86855159810715,-0.495598750427718,0.));
#2793=DIRECTION('',(0.,0.,-1.));
#2794=DIRECTION('center_axis',(0.,0.,1.));
#2795=DIRECTION('ref_axis',(0.86855159810715,-0.495598750427718,0.));
#2796=DIRECTION('center_axis',(0.,0.,1.));
#2797=DIRECTION('ref_axis',(0.491003386044519,0.871157663625143,0.));
#2798=DIRECTION('',(0.,0.,1.));
#2799=DIRECTION('center_axis',(0.,0.,1.));
#2800=DIRECTION('ref_axis',(0.491003386044519,0.871157663625143,0.));
#2801=DIRECTION('',(0.,0.,1.));
#2802=DIRECTION('center_axis',(0.,0.,-1.));
#2803=DIRECTION('ref_axis',(0.491003386044519,0.871157663625143,0.));
#2804=DIRECTION('center_axis',(0.,0.,1.));
#2805=DIRECTION('ref_axis',(-0.309016994374947,-0.951056516295154,0.));
#2806=DIRECTION('center_axis',(0.,0.,1.));
#2807=DIRECTION('ref_axis',(-1.,0.,0.));
#2808=DIRECTION('center_axis',(0.,0.,1.));
#2809=DIRECTION('ref_axis',(-0.99719862161961,0.0747991245934742,0.));
#2810=DIRECTION('center_axis',(0.,0.,-1.));
#2811=DIRECTION('ref_axis',(0.99503953924054,-0.0994802259143675,0.));
#2812=DIRECTION('center_axis',(0.,0.,1.));
#2813=DIRECTION('ref_axis',(-0.99719862161961,0.0747991245934742,0.));
#2814=DIRECTION('center_axis',(0.,0.,1.));
#2815=DIRECTION('ref_axis',(-0.99719862161961,0.0747991245934742,0.));
#2816=DIRECTION('',(0.,0.,1.));
#2817=DIRECTION('center_axis',(0.,0.,1.));
#2818=DIRECTION('ref_axis',(0.99503953924054,-0.0994802259143675,0.));
#2819=DIRECTION('',(0.,0.,-1.));
#2820=DIRECTION('center_axis',(0.,0.,1.));
#2821=DIRECTION('ref_axis',(0.99503953924054,-0.0994802259143675,0.));
#2822=DIRECTION('center_axis',(0.,0.,1.));
#2823=DIRECTION('ref_axis',(0.0942221693154581,0.995551195473889,0.));
#2824=DIRECTION('',(0.,0.,1.));
#2825=DIRECTION('center_axis',(0.,0.,1.));
#2826=DIRECTION('ref_axis',(0.0942221693154581,0.995551195473889,0.));
#2827=DIRECTION('',(0.,0.,1.));
#2828=DIRECTION('center_axis',(0.,0.,-1.));
#2829=DIRECTION('ref_axis',(0.0942221693154581,0.995551195473889,0.));
#2830=DIRECTION('center_axis',(0.,0.,1.));
#2831=DIRECTION('ref_axis',(0.104528463267654,-0.994521895368273,0.));
#2832=DIRECTION('center_axis',(0.,0.,1.));
#2833=DIRECTION('ref_axis',(-1.,0.,0.));
#2834=DIRECTION('center_axis',(0.,0.,1.));
#2835=DIRECTION('ref_axis',(-0.941409815990215,-0.337264819329364,0.));
#2836=DIRECTION('center_axis',(0.,0.,-1.));
#2837=DIRECTION('ref_axis',(0.949476104388814,0.313839333409058,0.));
#2838=DIRECTION('center_axis',(0.,0.,1.));
#2839=DIRECTION('ref_axis',(-0.941409815990215,-0.337264819329364,0.));
#2840=DIRECTION('center_axis',(0.,0.,1.));
#2841=DIRECTION('ref_axis',(-0.941409815990215,-0.337264819329364,0.));
#2842=DIRECTION('',(0.,0.,1.));
#2843=DIRECTION('center_axis',(0.,0.,1.));
#2844=DIRECTION('ref_axis',(0.949476104388814,0.313839333409058,0.));
#2845=DIRECTION('',(0.,0.,-1.));
#2846=DIRECTION('center_axis',(0.,0.,1.));
#2847=DIRECTION('ref_axis',(0.949476104388814,0.313839333409058,0.));
#2848=DIRECTION('center_axis',(0.,0.,1.));
#2849=DIRECTION('ref_axis',(-0.31885091646978,0.947804881326521,0.));
#2850=DIRECTION('',(0.,0.,1.));
#2851=DIRECTION('center_axis',(0.,0.,1.));
#2852=DIRECTION('ref_axis',(-0.31885091646978,0.947804881326521,0.));
#2853=DIRECTION('',(0.,0.,1.));
#2854=DIRECTION('center_axis',(0.,0.,-1.));
#2855=DIRECTION('ref_axis',(-0.31885091646978,0.947804881326521,0.));
#2856=DIRECTION('center_axis',(0.,0.,1.));
#2857=DIRECTION('ref_axis',(0.5,-0.866025403784438,0.));
#2858=DIRECTION('center_axis',(0.,0.,1.));
#2859=DIRECTION('ref_axis',(-1.,0.,0.));
#2860=DIRECTION('center_axis',(0.,0.,1.));
#2861=DIRECTION('ref_axis',(-0.722842700736426,-0.69101261203546,0.));
#2862=DIRECTION('center_axis',(0.,0.,-1.));
#2863=DIRECTION('ref_axis',(0.739739625368646,0.672893220845221,0.));
#2864=DIRECTION('center_axis',(0.,0.,1.));
#2865=DIRECTION('ref_axis',(-0.722842700736426,-0.69101261203546,0.));
#2866=DIRECTION('center_axis',(0.,0.,1.));
#2867=DIRECTION('ref_axis',(-0.722842700736426,-0.69101261203546,0.));
#2868=DIRECTION('',(0.,0.,1.));
#2869=DIRECTION('center_axis',(0.,0.,1.));
#2870=DIRECTION('ref_axis',(0.739739625368646,0.672893220845221,0.));
#2871=DIRECTION('',(0.,0.,-1.));
#2872=DIRECTION('center_axis',(0.,0.,1.));
#2873=DIRECTION('ref_axis',(0.739739625368646,0.672893220845221,0.));
#2874=DIRECTION('center_axis',(0.,0.,1.));
#2875=DIRECTION('ref_axis',(-0.676791782127754,0.736174492660767,0.));
#2876=DIRECTION('',(0.,0.,1.));
#2877=DIRECTION('center_axis',(0.,0.,1.));
#2878=DIRECTION('ref_axis',(-0.676791782127754,0.736174492660767,0.));
#2879=DIRECTION('',(0.,0.,1.));
#2880=DIRECTION('center_axis',(0.,0.,-1.));
#2881=DIRECTION('ref_axis',(-0.676791782127754,0.736174492660767,0.));
#2882=DIRECTION('center_axis',(0.,0.,1.));
#2883=DIRECTION('ref_axis',(0.809016994374948,-0.587785252292473,0.));
#2884=DIRECTION('center_axis',(0.,0.,1.));
#2885=DIRECTION('ref_axis',(-1.,0.,0.));
#2886=DIRECTION('center_axis',(0.,0.,1.));
#2887=DIRECTION('ref_axis',(-0.379289515705529,-0.925278046468123,0.));
#2888=DIRECTION('center_axis',(0.,0.,-1.));
#2889=DIRECTION('ref_axis',(0.402095444798718,0.915597757354244,0.));
#2890=DIRECTION('center_axis',(0.,0.,1.));
#2891=DIRECTION('ref_axis',(-0.379289515705529,-0.925278046468123,0.));
#2892=DIRECTION('center_axis',(0.,0.,1.));
#2893=DIRECTION('ref_axis',(-0.379289515705529,-0.925278046468123,0.));
#2894=DIRECTION('',(0.,0.,1.));
#2895=DIRECTION('center_axis',(0.,0.,1.));
#2896=DIRECTION('ref_axis',(0.402095444798718,0.915597757354244,0.));
#2897=DIRECTION('',(0.,0.,-1.));
#2898=DIRECTION('center_axis',(0.,0.,1.));
#2899=DIRECTION('ref_axis',(0.402095444798718,0.915597757354244,0.));
#2900=DIRECTION('center_axis',(0.,0.,1.));
#2901=DIRECTION('ref_axis',(-0.917709200195522,0.397252846278659,0.));
#2902=DIRECTION('',(0.,0.,1.));
#2903=DIRECTION('center_axis',(0.,0.,1.));
#2904=DIRECTION('ref_axis',(-0.917709200195522,0.397252846278659,0.));
#2905=DIRECTION('',(0.,0.,1.));
#2906=DIRECTION('center_axis',(0.,0.,-1.));
#2907=DIRECTION('ref_axis',(-0.917709200195522,0.397252846278659,0.));
#2908=DIRECTION('center_axis',(0.,0.,1.));
#2909=DIRECTION('ref_axis',(0.978147600733806,-0.207911690817759,0.));
#2910=DIRECTION('center_axis',(0.,0.,1.));
#2911=DIRECTION('ref_axis',(-1.,0.,0.));
#2912=DIRECTION('center_axis',(0.,0.,1.));
#2913=DIRECTION('ref_axis',(0.0298462723279306,-0.999554500779286,0.));
#2914=DIRECTION('center_axis',(0.,0.,-1.));
#2915=DIRECTION('ref_axis',(-0.00507469109934694,0.999987123672223,0.));
#2916=DIRECTION('center_axis',(0.,0.,1.));
#2917=DIRECTION('ref_axis',(0.0298462723279306,-0.999554500779286,0.));
#2918=DIRECTION('center_axis',(0.,0.,1.));
#2919=DIRECTION('ref_axis',(0.0298462723279306,-0.999554500779286,0.));
#2920=DIRECTION('',(0.,0.,1.));
#2921=DIRECTION('center_axis',(0.,0.,1.));
#2922=DIRECTION('ref_axis',(-0.00507469109934694,0.999987123672223,0.));
#2923=DIRECTION('',(0.,0.,-1.));
#2924=DIRECTION('center_axis',(0.,0.,1.));
#2925=DIRECTION('ref_axis',(-0.00507469109934694,0.999987123672223,0.));
#2926=DIRECTION('center_axis',(0.,0.,1.));
#2927=DIRECTION('ref_axis',(-0.999946360423132,-0.0103574261538407,0.));
#2928=DIRECTION('',(0.,0.,1.));
#2929=DIRECTION('center_axis',(0.,0.,1.));
#2930=DIRECTION('ref_axis',(-0.999946360423132,-0.0103574261538407,0.));
#2931=DIRECTION('',(0.,0.,1.));
#2932=DIRECTION('center_axis',(0.,0.,-1.));
#2933=DIRECTION('ref_axis',(-0.999946360423132,-0.0103574261538407,0.));
#2934=DIRECTION('center_axis',(0.,0.,1.));
#2935=DIRECTION('ref_axis',(0.978147600733805,0.20791169081776,0.));
#2936=DIRECTION('center_axis',(0.,0.,1.));
#2937=DIRECTION('ref_axis',(-1.,0.,0.));
#2938=DIRECTION('center_axis',(0.,0.,1.));
#2939=DIRECTION('ref_axis',(0.433821368731019,-0.900998901238145,0.));
#2940=DIRECTION('center_axis',(0.,0.,-1.));
#2941=DIRECTION('ref_axis',(-0.411367366804213,0.911469631709454,0.));
#2942=DIRECTION('center_axis',(0.,0.,1.));
#2943=DIRECTION('ref_axis',(0.433821368731019,-0.900998901238145,0.));
#2944=DIRECTION('center_axis',(0.,0.,1.));
#2945=DIRECTION('ref_axis',(0.433821368731019,-0.900998901238145,0.));
#2946=DIRECTION('',(0.,0.,1.));
#2947=DIRECTION('center_axis',(0.,0.,1.));
#2948=DIRECTION('ref_axis',(-0.411367366804213,0.911469631709454,0.));
#2949=DIRECTION('',(0.,0.,-1.));
#2950=DIRECTION('center_axis',(0.,0.,1.));
#2951=DIRECTION('ref_axis',(-0.411367366804213,0.911469631709454,0.));
#2952=DIRECTION('center_axis',(0.,0.,1.));
#2953=DIRECTION('ref_axis',(-0.909283710706085,-0.416176805510078,0.));
#2954=DIRECTION('',(0.,0.,1.));
#2955=DIRECTION('center_axis',(0.,0.,1.));
#2956=DIRECTION('ref_axis',(-0.909283710706085,-0.416176805510078,0.));
#2957=DIRECTION('',(0.,0.,1.));
#2958=DIRECTION('center_axis',(0.,0.,-1.));
#2959=DIRECTION('ref_axis',(-0.909283710706085,-0.416176805510078,0.));
#2960=DIRECTION('center_axis',(0.,0.,1.));
#2961=DIRECTION('ref_axis',(0.809016994374947,0.587785252292473,0.));
#2962=DIRECTION('center_axis',(0.,0.,1.));
#2963=DIRECTION('ref_axis',(-1.,0.,0.));
#2964=DIRECTION('center_axis',(0.,0.,1.));
#2965=DIRECTION('ref_axis',(0.762784809337106,-0.646652406354879,0.));
#2966=DIRECTION('center_axis',(0.,0.,-1.));
#2967=DIRECTION('ref_axis',(-0.746530887633426,0.66535075998247,0.));
#2968=DIRECTION('center_axis',(0.,0.,1.));
#2969=DIRECTION('ref_axis',(0.762784809337106,-0.646652406354879,0.));
#2970=DIRECTION('center_axis',(0.,0.,1.));
#2971=DIRECTION('ref_axis',(0.762784809337106,-0.646652406354879,0.));
#2972=DIRECTION('',(0.,0.,1.));
#2973=DIRECTION('center_axis',(0.,0.,1.));
#2974=DIRECTION('ref_axis',(-0.746530887633426,0.66535075998247,0.));
#2975=DIRECTION('',(0.,0.,-1.));
#2976=DIRECTION('center_axis',(0.,0.,1.));
#2977=DIRECTION('ref_axis',(-0.746530887633426,0.66535075998247,0.));
#2978=DIRECTION('center_axis',(0.,0.,1.));
#2979=DIRECTION('ref_axis',(-0.661397646824773,-0.75003543434604,0.));
#2980=DIRECTION('',(0.,0.,1.));
#2981=DIRECTION('center_axis',(0.,0.,1.));
#2982=DIRECTION('ref_axis',(-0.661397646824773,-0.75003543434604,0.));
#2983=DIRECTION('',(0.,0.,1.));
#2984=DIRECTION('center_axis',(0.,0.,-1.));
#2985=DIRECTION('ref_axis',(-0.661397646824773,-0.75003543434604,0.));
#2986=DIRECTION('center_axis',(0.,0.,1.));
#2987=DIRECTION('ref_axis',(0.5,0.866025403784439,0.));
#2988=DIRECTION('center_axis',(0.,0.,1.));
#2989=DIRECTION('ref_axis',(-1.,0.,0.));
#2990=DIRECTION('center_axis',(0.,0.,1.));
#2991=DIRECTION('ref_axis',(0.959855826726362,-0.280493835760168,0.));
#2992=DIRECTION('center_axis',(0.,0.,-1.));
#2993=DIRECTION('ref_axis',(-0.952612435970617,0.30418669733262,0.));
#2994=DIRECTION('center_axis',(0.,0.,1.));
#2995=DIRECTION('ref_axis',(0.959855826726362,-0.280493835760168,0.));
#2996=DIRECTION('center_axis',(0.,0.,1.));
#2997=DIRECTION('ref_axis',(0.959855826726362,-0.280493835760168,0.));
#2998=DIRECTION('',(0.,0.,1.));
#2999=DIRECTION('center_axis',(0.,0.,1.));
#3000=DIRECTION('ref_axis',(-0.952612435970617,0.30418669733262,0.));
#3001=DIRECTION('',(0.,0.,-1.));
#3002=DIRECTION('center_axis',(0.,0.,1.));
#3003=DIRECTION('ref_axis',(-0.952612435970617,0.30418669733262,0.));
#3004=DIRECTION('center_axis',(0.,0.,1.));
#3005=DIRECTION('ref_axis',(-0.299149921198468,-0.954206122725562,0.));
#3006=DIRECTION('',(0.,0.,1.));
#3007=DIRECTION('center_axis',(0.,0.,1.));
#3008=DIRECTION('ref_axis',(-0.299149921198468,-0.954206122725562,0.));
#3009=DIRECTION('',(0.,0.,1.));
#3010=DIRECTION('center_axis',(0.,0.,-1.));
#3011=DIRECTION('ref_axis',(-0.299149921198468,-0.954206122725562,0.));
#3012=DIRECTION('center_axis',(0.,0.,1.));
#3013=DIRECTION('ref_axis',(0.104528463267653,0.994521895368273,0.));
#3014=DIRECTION('center_axis',(0.,0.,1.));
#3015=DIRECTION('ref_axis',(-1.,0.,0.));
#3016=DIRECTION('center_axis',(0.,0.,1.));
#3017=DIRECTION('ref_axis',(0.990959051658197,0.134164667243976,0.));
#3018=DIRECTION('center_axis',(0.,0.,-1.));
#3019=DIRECTION('ref_axis',(-0.993978639916195,-0.109574008735429,0.));
#3020=DIRECTION('center_axis',(0.,0.,1.));
#3021=DIRECTION('ref_axis',(0.990959051658197,0.134164667243976,0.));
#3022=DIRECTION('center_axis',(0.,0.,1.));
#3023=DIRECTION('ref_axis',(0.990959051658197,0.134164667243976,0.));
#3024=DIRECTION('',(0.,0.,1.));
#3025=DIRECTION('center_axis',(0.,0.,1.));
#3026=DIRECTION('ref_axis',(-0.993978639916195,-0.109574008735429,0.));
#3027=DIRECTION('',(0.,0.,-1.));
#3028=DIRECTION('center_axis',(0.,0.,1.));
#3029=DIRECTION('ref_axis',(-0.993978639916195,-0.109574008735429,0.));
#3030=DIRECTION('center_axis',(0.,0.,1.));
#3031=DIRECTION('ref_axis',(0.114823543494768,-0.99338590379535,0.));
#3032=DIRECTION('',(0.,0.,1.));
#3033=DIRECTION('center_axis',(0.,0.,1.));
#3034=DIRECTION('ref_axis',(0.114823543494768,-0.99338590379535,0.));
#3035=DIRECTION('',(0.,0.,1.));
#3036=DIRECTION('center_axis',(0.,0.,-1.));
#3037=DIRECTION('ref_axis',(0.114823543494768,-0.99338590379535,0.));
#3038=DIRECTION('center_axis',(0.,0.,1.));
#3039=DIRECTION('ref_axis',(-0.309016994374947,0.951056516295154,0.));
#3040=DIRECTION('center_axis',(0.,0.,1.));
#3041=DIRECTION('ref_axis',(-1.,0.,0.));
#3042=DIRECTION('center_axis',(0.,0.,1.));
#3043=DIRECTION('ref_axis',(0.850716453977969,0.525624880433899,0.));
#3044=DIRECTION('center_axis',(0.,0.,-1.));
#3045=DIRECTION('ref_axis',(-0.863476907007803,-0.504388373244505,0.));
#3046=DIRECTION('center_axis',(0.,0.,1.));
#3047=DIRECTION('ref_axis',(0.850716453977969,0.525624880433899,0.));
#3048=DIRECTION('center_axis',(0.,0.,1.));
#3049=DIRECTION('ref_axis',(0.850716453977969,0.525624880433899,0.));
#3050=DIRECTION('',(0.,0.,1.));
#3051=DIRECTION('center_axis',(0.,0.,1.));
#3052=DIRECTION('ref_axis',(-0.863476907007803,-0.504388373244505,0.));
#3053=DIRECTION('',(0.,0.,-1.));
#3054=DIRECTION('center_axis',(0.,0.,1.));
#3055=DIRECTION('ref_axis',(-0.863476907007803,-0.504388373244505,0.));
#3056=DIRECTION('center_axis',(0.,0.,1.));
#3057=DIRECTION('ref_axis',(0.508942974378613,-0.860800237471302,0.));
#3058=DIRECTION('',(0.,0.,1.));
#3059=DIRECTION('center_axis',(0.,0.,1.));
#3060=DIRECTION('ref_axis',(0.508942974378613,-0.860800237471302,0.));
#3061=DIRECTION('',(0.,0.,1.));
#3062=DIRECTION('center_axis',(0.,0.,-1.));
#3063=DIRECTION('ref_axis',(0.508942974378613,-0.860800237471302,0.));
#3064=DIRECTION('center_axis',(0.,0.,1.));
#3065=DIRECTION('ref_axis',(-0.669130606358858,0.743144825477394,0.));
#3066=DIRECTION('center_axis',(0.,0.,1.));
#3067=DIRECTION('ref_axis',(-1.,0.,0.));
#3068=DIRECTION('center_axis',(0.,0.,1.));
#3069=DIRECTION('ref_axis',(0.563377252888591,0.826199776644671,0.));
#3070=DIRECTION('center_axis',(0.,0.,-1.));
#3071=DIRECTION('ref_axis',(-0.583672172436327,-0.811989405795087,0.));
#3072=DIRECTION('center_axis',(0.,0.,1.));
#3073=DIRECTION('ref_axis',(0.563377252888591,0.826199776644671,0.));
#3074=DIRECTION('center_axis',(0.,0.,1.));
#3075=DIRECTION('ref_axis',(0.563377252888591,0.826199776644671,0.));
#3076=DIRECTION('',(0.,0.,1.));
#3077=DIRECTION('center_axis',(0.,0.,1.));
#3078=DIRECTION('ref_axis',(-0.583672172436327,-0.811989405795087,0.));
#3079=DIRECTION('',(0.,0.,-1.));
#3080=DIRECTION('center_axis',(0.,0.,1.));
#3081=DIRECTION('ref_axis',(-0.583672172436327,-0.811989405795087,0.));
#3082=DIRECTION('center_axis',(0.,0.,1.));
#3083=DIRECTION('ref_axis',(0.815061541390626,-0.57937438996381,0.));
#3084=DIRECTION('',(0.,0.,1.));
#3085=DIRECTION('center_axis',(0.,0.,1.));
#3086=DIRECTION('ref_axis',(0.815061541390626,-0.57937438996381,0.));
#3087=DIRECTION('',(0.,0.,1.));
#3088=DIRECTION('center_axis',(0.,0.,-1.));
#3089=DIRECTION('ref_axis',(0.815061541390626,-0.57937438996381,0.));
#3090=DIRECTION('center_axis',(0.,0.,1.));
#3091=DIRECTION('ref_axis',(-0.913545457642601,0.4067366430758,0.));
#3092=DIRECTION('center_axis',(0.,0.,1.));
#3093=DIRECTION('ref_axis',(-1.,0.,0.));
#3094=DIRECTION('center_axis',(0.,0.,1.));
#3095=DIRECTION('ref_axis',(0.17862500665311,0.983917225684242,0.));
#3096=DIRECTION('center_axis',(0.,0.,-1.));
#3097=DIRECTION('ref_axis',(-0.202945216755389,-0.979190093391528,0.));
#3098=DIRECTION('center_axis',(0.,0.,1.));
#3099=DIRECTION('ref_axis',(0.17862500665311,0.983917225684242,0.));
#3100=DIRECTION('center_axis',(0.,0.,1.));
#3101=DIRECTION('ref_axis',(0.17862500665311,0.983917225684242,0.));
#3102=DIRECTION('',(0.,0.,1.));
#3103=DIRECTION('center_axis',(0.,0.,1.));
#3104=DIRECTION('ref_axis',(-0.202945216755389,-0.979190093391528,0.));
#3105=DIRECTION('',(0.,0.,-1.));
#3106=DIRECTION('center_axis',(0.,0.,1.));
#3107=DIRECTION('ref_axis',(-0.202945216755389,-0.979190093391528,0.));
#3108=DIRECTION('center_axis',(0.,0.,-1.));
#3109=DIRECTION('ref_axis',(-1.,0.,0.));
#3110=DIRECTION('center_axis',(0.,0.,1.));
#3111=DIRECTION('ref_axis',(-1.,0.,0.));
#3112=DIRECTION('',(0.,0.,1.));
#3113=DIRECTION('center_axis',(0.,0.,-1.));
#3114=DIRECTION('ref_axis',(1.,0.,0.));
#3115=DIRECTION('center_axis',(0.,0.,1.));
#3116=DIRECTION('ref_axis',(-1.,0.,0.));
#3117=DIRECTION('',(0.,0.,-1.));
#3118=DIRECTION('center_axis',(0.,0.,-1.));
#3119=DIRECTION('ref_axis',(1.,0.,0.));
#3120=DIRECTION('center_axis',(0.,0.,-1.));
#3121=DIRECTION('ref_axis',(1.,0.,0.));
#3122=DIRECTION('center_axis',(0.,0.,-1.));
#3123=DIRECTION('ref_axis',(1.,0.,0.));
#3124=DIRECTION('center_axis',(0.,0.,-1.));
#3125=DIRECTION('ref_axis',(1.,0.,0.));
#3126=DIRECTION('center_axis',(0.,0.,-1.));
#3127=DIRECTION('ref_axis',(1.,0.,0.));
#3128=DIRECTION('center_axis',(0.,0.,-1.));
#3129=DIRECTION('ref_axis',(1.,0.,0.));
#3130=DIRECTION('center_axis',(0.,0.,-1.));
#3131=DIRECTION('ref_axis',(1.,0.,0.));
#3132=DIRECTION('center_axis',(0.,0.,-1.));
#3133=DIRECTION('ref_axis',(1.,0.,0.));
#3134=DIRECTION('center_axis',(0.,0.,-1.));
#3135=DIRECTION('ref_axis',(1.,0.,0.));
#3136=DIRECTION('center_axis',(0.,0.,-1.));
#3137=DIRECTION('ref_axis',(1.,0.,0.));
#3138=DIRECTION('center_axis',(0.,0.,-1.));
#3139=DIRECTION('ref_axis',(1.,0.,0.));
#3140=DIRECTION('center_axis',(0.,0.,-1.));
#3141=DIRECTION('ref_axis',(1.,0.,0.));
#3142=DIRECTION('center_axis',(0.,0.,-1.));
#3143=DIRECTION('ref_axis',(1.,0.,0.));
#3144=DIRECTION('center_axis',(0.,0.,-1.));
#3145=DIRECTION('ref_axis',(1.,0.,0.));
#3146=DIRECTION('center_axis',(0.,0.,-1.));
#3147=DIRECTION('ref_axis',(1.,0.,0.));
#3148=DIRECTION('',(0.,0.,1.));
#3149=DIRECTION('center_axis',(0.,0.,1.));
#3150=DIRECTION('ref_axis',(0.980248563294553,-0.197769446980481,0.));
#3151=DIRECTION('center_axis',(0.,0.,1.));
#3152=DIRECTION('ref_axis',(0.980248563294553,-0.197769446980481,0.));
#3153=DIRECTION('',(0.,0.,1.));
#3154=DIRECTION('center_axis',(0.,0.,-1.));
#3155=DIRECTION('ref_axis',(0.980248563294553,-0.197769446980481,0.));
#3156=DIRECTION('center_axis',(0.,0.,1.));
#3157=DIRECTION('ref_axis',(-1.,0.,0.));
#3158=DIRECTION('center_axis',(0.,0.,1.));
#3159=DIRECTION('ref_axis',(-0.237013125989935,0.971506447795628,0.));
#3160=DIRECTION('center_axis',(0.,0.,-1.));
#3161=DIRECTION('ref_axis',(0.212872810601971,-0.977079918177841,0.));
#3162=DIRECTION('center_axis',(0.,0.,1.));
#3163=DIRECTION('ref_axis',(-0.237013125989935,0.971506447795628,0.));
#3164=DIRECTION('center_axis',(0.,0.,1.));
#3165=DIRECTION('ref_axis',(-0.237013125989935,0.971506447795628,0.));
#3166=DIRECTION('',(0.,0.,1.));
#3167=DIRECTION('center_axis',(0.,0.,1.));
#3168=DIRECTION('ref_axis',(0.212872810601971,-0.977079918177841,0.));
#3169=DIRECTION('center_axis',(0.,0.,1.));
#3170=DIRECTION('ref_axis',(0.212872810601971,-0.977079918177841,0.));
#3171=DIRECTION('center_axis',(0.,0.,-1.));
#3172=DIRECTION('ref_axis',(-1.,0.,0.));
#3173=DIRECTION('center_axis',(0.,0.,-1.));
#3174=DIRECTION('ref_axis',(1.,0.,0.));
#3175=DIRECTION('center_axis',(0.,0.,1.));
#3176=DIRECTION('ref_axis',(1.,0.,0.));
#3177=DIRECTION('center_axis',(0.,0.,-1.));
#3178=DIRECTION('ref_axis',(1.,0.,0.));
#3179=DIRECTION('center_axis',(0.,0.,-1.));
#3180=DIRECTION('ref_axis',(-1.,0.,0.));
#3181=DIRECTION('center_axis',(0.,0.,-1.));
#3182=DIRECTION('ref_axis',(1.,0.,0.));
#3183=DIRECTION('',(-0.709089650734988,8.68384371081118E-17,0.705118335615046));
#3184=DIRECTION('center_axis',(0.,0.,-1.));
#3185=DIRECTION('ref_axis',(-1.,0.,0.));
#3186=DIRECTION('center_axis',(0.,0.,-1.));
#3187=DIRECTION('ref_axis',(1.,0.,0.));
#3188=DIRECTION('',(0.,0.,1.));
#3189=DIRECTION('',(0.,0.,1.));
#3190=DIRECTION('center_axis',(0.,0.,1.));
#3191=DIRECTION('ref_axis',(-1.,0.,0.));
#3192=DIRECTION('',(-0.705118335615046,-8.63520912731075E-17,-0.709089650734988));
#3193=DIRECTION('center_axis',(0.,0.,-1.));
#3194=DIRECTION('ref_axis',(1.,0.,0.));
#3195=DIRECTION('center_axis',(0.,0.,-1.));
#3196=DIRECTION('ref_axis',(-1.,0.,0.));
#3197=DIRECTION('center_axis',(0.,0.,-1.));
#3198=DIRECTION('ref_axis',(1.,0.,0.));
#3199=DIRECTION('center_axis',(0.,0.,-1.));
#3200=DIRECTION('ref_axis',(-1.,0.,0.));
#3201=DIRECTION('center_axis',(0.,0.,-1.));
#3202=DIRECTION('ref_axis',(1.,0.,0.));
#3203=DIRECTION('',(0.799712036156634,-9.79364785318835E-17,-0.600383759962084));
#3204=DIRECTION('center_axis',(0.,0.,1.));
#3205=DIRECTION('ref_axis',(-1.,0.,0.));
#3206=DIRECTION('',(-0.795904561203624,-9.74701973304796E-17,-0.605422108495608));
#3207=DIRECTION('center_axis',(0.,0.,-1.));
#3208=DIRECTION('ref_axis',(1.,0.,0.));
#3209=DIRECTION('center_axis',(0.,0.,-1.));
#3210=DIRECTION('ref_axis',(-1.,0.,0.));
#3211=DIRECTION('center_axis',(0.,0.,-1.));
#3212=DIRECTION('ref_axis',(1.,0.,0.));
#3213=DIRECTION('center_axis',(0.,0.,-1.));
#3214=DIRECTION('ref_axis',(-1.,0.,0.));
#3215=DIRECTION('',(0.710031613960551,-8.69537943330218E-17,-0.704169799960617));
#3216=DIRECTION('center_axis',(0.,0.,1.));
#3217=DIRECTION('ref_axis',(-1.,0.,0.));
#3218=DIRECTION('',(0.704169799960617,8.62359291578001E-17,0.710031613960551));
#3219=DIRECTION('center_axis',(0.,0.,-1.));
#3220=DIRECTION('ref_axis',(1.,0.,0.));
#3221=DIRECTION('center_axis',(0.,0.,1.));
#3222=DIRECTION('ref_axis',(1.,0.,0.));
#3223=DIRECTION('center_axis',(0.,0.,-1.));
#3224=DIRECTION('ref_axis',(1.,0.,0.));
#3225=DIRECTION('center_axis',(0.,0.,-1.));
#3226=DIRECTION('ref_axis',(-1.,0.,0.));
#3227=DIRECTION('center_axis',(0.,0.,-1.));
#3228=DIRECTION('ref_axis',(1.,0.,0.));
#3229=DIRECTION('',(-0.790648054928562,9.68264609720345E-17,0.612270898571605));
#3230=DIRECTION('center_axis',(0.,0.,1.));
#3231=DIRECTION('ref_axis',(-1.,0.,0.));
#3232=DIRECTION('',(0.802697028722426,9.8302034691001E-17,0.596387022058821));
#3233=DIRECTION('center_axis',(0.,0.,-1.));
#3234=DIRECTION('ref_axis',(1.,0.,0.));
#3235=DIRECTION('center_axis',(0.,0.,1.));
#3236=DIRECTION('ref_axis',(1.,0.,0.));
#3237=DIRECTION('center_axis',(0.,0.,-1.));
#3238=DIRECTION('ref_axis',(1.,0.,0.));
#3239=DIRECTION('center_axis',(0.,0.,-1.));
#3240=DIRECTION('ref_axis',(-1.,0.,0.));
#3241=DIRECTION('center_axis',(0.,0.,-1.));
#3242=DIRECTION('ref_axis',(1.,0.,0.));
#3243=DIRECTION('',(-0.699050213581169,8.56089606505452E-17,0.715072582953732));
#3244=DIRECTION('center_axis',(0.,0.,-1.));
#3245=DIRECTION('ref_axis',(-1.,0.,0.));
#3246=DIRECTION('center_axis',(0.,0.,-1.));
#3247=DIRECTION('ref_axis',(1.,0.,0.));
#3248=DIRECTION('',(0.,0.,1.));
#3249=DIRECTION('center_axis',(0.,0.,1.));
#3250=DIRECTION('ref_axis',(-1.,0.,0.));
#3251=DIRECTION('',(-0.715072582953733,-8.75711349872319E-17,-0.699050213581168));
#3252=DIRECTION('axis',(0.,0.,1.));
#3253=DIRECTION('refdir',(1.,0.,0.));
#3254=DIRECTION('center_axis',(1.,0.,0.));
#3255=DIRECTION('ref_axis',(0.,1.,4.63931189975154E-15));
#3256=DIRECTION('',(-1.,0.,0.));
#3257=DIRECTION('center_axis',(-1.,0.,0.));
#3258=DIRECTION('ref_axis',(0.,1.,4.63931189975154E-15));
#3259=DIRECTION('center_axis',(1.,0.,0.));
#3260=DIRECTION('ref_axis',(0.,1.,4.63931189975154E-15));
#3261=DIRECTION('',(-1.,0.,0.));
#3262=DIRECTION('center_axis',(1.,0.,0.));
#3263=DIRECTION('ref_axis',(0.,1.,4.63931189975154E-15));
#3264=DIRECTION('',(-1.,0.,0.));
#3265=DIRECTION('center_axis',(1.,0.,0.));
#3266=DIRECTION('ref_axis',(0.,1.,4.63931189975154E-15));
#3267=DIRECTION('',(-1.,0.,0.));
#3268=DIRECTION('center_axis',(1.,0.,0.));
#3269=DIRECTION('ref_axis',(0.,1.,4.63931189975154E-15));
#3270=DIRECTION('',(-1.,0.,0.));
#3271=DIRECTION('center_axis',(1.,0.,0.));
#3272=DIRECTION('ref_axis',(0.,1.,4.63931189975154E-15));
#3273=DIRECTION('',(-1.,0.,0.));
#3274=DIRECTION('center_axis',(1.,0.,0.));
#3275=DIRECTION('ref_axis',(0.,1.,0.));
#3276=DIRECTION('',(-1.,0.,0.));
#3277=DIRECTION('center_axis',(-1.,0.,0.));
#3278=DIRECTION('ref_axis',(0.,1.,0.));
#3279=DIRECTION('center_axis',(1.,0.,0.));
#3280=DIRECTION('ref_axis',(0.,1.,0.));
#3281=DIRECTION('',(-1.,0.,0.));
#3282=DIRECTION('center_axis',(1.,0.,0.));
#3283=DIRECTION('ref_axis',(0.,1.,0.));
#3284=DIRECTION('',(-1.,0.,0.));
#3285=DIRECTION('center_axis',(1.,0.,0.));
#3286=DIRECTION('ref_axis',(0.,1.,0.));
#3287=DIRECTION('',(-1.,0.,0.));
#3288=DIRECTION('center_axis',(1.,0.,0.));
#3289=DIRECTION('ref_axis',(0.,1.,0.));
#3290=DIRECTION('',(-1.,0.,0.));
#3291=DIRECTION('center_axis',(1.,0.,0.));
#3292=DIRECTION('ref_axis',(0.,1.,0.));
#3293=DIRECTION('',(-1.,0.,0.));
#3294=DIRECTION('center_axis',(1.,0.,0.));
#3295=DIRECTION('ref_axis',(0.,1.,0.));
#3296=DIRECTION('center_axis',(-1.,0.,0.));
#3297=DIRECTION('ref_axis',(0.,1.,0.));
#3298=DIRECTION('center_axis',(1.,0.,0.));
#3299=DIRECTION('ref_axis',(0.,1.,4.63931189975154E-15));
#3300=DIRECTION('center_axis',(1.,0.,0.));
#3301=DIRECTION('ref_axis',(0.,1.,4.63931189975154E-15));
#3302=DIRECTION('center_axis',(1.,0.,0.));
#3303=DIRECTION('ref_axis',(0.,1.,0.));
#3304=DIRECTION('',(0.,0.5,0.866025403784439));
#3305=DIRECTION('',(0.,1.,0.));
#3306=DIRECTION('',(0.,0.499999999999999,-0.866025403784439));
#3307=DIRECTION('',(0.,-0.5,-0.866025403784438));
#3308=DIRECTION('',(0.,-1.,4.80740671595891E-16));
#3309=DIRECTION('',(0.,-0.499999999999999,0.866025403784439));
#3310=DIRECTION('center_axis',(0.,-0.866025403784439,0.5));
#3311=DIRECTION('ref_axis',(0.,0.5,0.866025403784439));
#3312=DIRECTION('',(-1.,0.,0.));
#3313=DIRECTION('',(0.,0.5,0.866025403784439));
#3314=DIRECTION('',(-1.,0.,0.));
#3315=DIRECTION('center_axis',(0.,-0.866025403784439,-0.499999999999999));
#3316=DIRECTION('ref_axis',(0.,-0.499999999999999,0.866025403784439));
#3317=DIRECTION('',(-1.,0.,0.));
#3318=DIRECTION('',(0.,-0.499999999999999,0.866025403784439));
#3319=DIRECTION('center_axis',(0.,-4.80740671595891E-16,-1.));
#3320=DIRECTION('ref_axis',(0.,-1.,4.80740671595891E-16));
#3321=DIRECTION('',(-1.,0.,0.));
#3322=DIRECTION('',(0.,-1.,4.80740671595891E-16));
#3323=DIRECTION('center_axis',(0.,0.866025403784438,-0.5));
#3324=DIRECTION('ref_axis',(0.,-0.5,-0.866025403784438));
#3325=DIRECTION('',(-1.,0.,0.));
#3326=DIRECTION('',(0.,-0.5,-0.866025403784438));
#3327=DIRECTION('center_axis',(0.,0.866025403784439,0.499999999999999));
#3328=DIRECTION('ref_axis',(0.,0.499999999999999,-0.866025403784439));
#3329=DIRECTION('',(-1.,0.,0.));
#3330=DIRECTION('',(0.,0.499999999999999,-0.866025403784439));
#3331=DIRECTION('center_axis',(0.,0.,1.));
#3332=DIRECTION('ref_axis',(0.,1.,0.));
#3333=DIRECTION('',(0.,1.,0.));
#3334=DIRECTION('center_axis',(-1.,0.,0.));
#3335=DIRECTION('ref_axis',(0.,0.,1.));
#3336=DIRECTION('center_axis',(1.,0.,0.));
#3337=DIRECTION('ref_axis',(0.,1.,0.));
#3338=DIRECTION('axis',(0.,0.,1.));
#3339=DIRECTION('refdir',(1.,0.,0.));
#3340=DIRECTION('center_axis',(-2.22044604925031E-16,1.,0.));
#3341=DIRECTION('ref_axis',(-1.,-2.22044604925031E-16,4.63931189975154E-15));
#3342=DIRECTION('',(2.22044604925031E-16,-1.,0.));
#3343=DIRECTION('center_axis',(2.22044604925031E-16,-1.,0.));
#3344=DIRECTION('ref_axis',(-1.,-2.22044604925031E-16,4.63931189975154E-15));
#3345=DIRECTION('center_axis',(-2.22044604925031E-16,1.,0.));
#3346=DIRECTION('ref_axis',(-1.,-2.22044604925031E-16,4.63931189975154E-15));
#3347=DIRECTION('',(2.22044604925031E-16,-1.,0.));
#3348=DIRECTION('center_axis',(-2.22044604925031E-16,1.,0.));
#3349=DIRECTION('ref_axis',(-1.,-2.22044604925031E-16,4.63931189975154E-15));
#3350=DIRECTION('',(2.22044604925031E-16,-1.,0.));
#3351=DIRECTION('center_axis',(-2.22044604925031E-16,1.,0.));
#3352=DIRECTION('ref_axis',(-1.,-2.22044604925031E-16,4.63931189975154E-15));
#3353=DIRECTION('',(2.22044604925031E-16,-1.,0.));
#3354=DIRECTION('center_axis',(-2.22044604925031E-16,1.,0.));
#3355=DIRECTION('ref_axis',(-1.,-2.22044604925031E-16,4.63931189975154E-15));
#3356=DIRECTION('',(2.22044604925031E-16,-1.,0.));
#3357=DIRECTION('center_axis',(-2.22044604925031E-16,1.,0.));
#3358=DIRECTION('ref_axis',(-1.,-2.22044604925031E-16,4.63931189975154E-15));
#3359=DIRECTION('',(2.22044604925031E-16,-1.,0.));
#3360=DIRECTION('center_axis',(-2.22044604925031E-16,1.,0.));
#3361=DIRECTION('ref_axis',(-1.,-2.22044604925031E-16,0.));
#3362=DIRECTION('',(2.22044604925031E-16,-1.,0.));
#3363=DIRECTION('center_axis',(2.22044604925031E-16,-1.,0.));
#3364=DIRECTION('ref_axis',(-1.,-2.22044604925031E-16,0.));
#3365=DIRECTION('center_axis',(-2.22044604925031E-16,1.,0.));
#3366=DIRECTION('ref_axis',(-1.,-2.22044604925031E-16,0.));
#3367=DIRECTION('',(2.22044604925031E-16,-1.,0.));
#3368=DIRECTION('center_axis',(-2.22044604925031E-16,1.,0.));
#3369=DIRECTION('ref_axis',(-1.,-2.22044604925031E-16,0.));
#3370=DIRECTION('',(2.22044604925031E-16,-1.,0.));
#3371=DIRECTION('center_axis',(-2.22044604925031E-16,1.,0.));
#3372=DIRECTION('ref_axis',(-1.,-2.22044604925031E-16,0.));
#3373=DIRECTION('',(2.22044604925031E-16,-1.,0.));
#3374=DIRECTION('center_axis',(-2.22044604925031E-16,1.,0.));
#3375=DIRECTION('ref_axis',(-1.,-2.22044604925031E-16,0.));
#3376=DIRECTION('',(2.22044604925031E-16,-1.,0.));
#3377=DIRECTION('center_axis',(-2.22044604925031E-16,1.,0.));
#3378=DIRECTION('ref_axis',(-1.,-2.22044604925031E-16,0.));
#3379=DIRECTION('',(2.22044604925031E-16,-1.,0.));
#3380=DIRECTION('center_axis',(-2.22044604925031E-16,1.,0.));
#3381=DIRECTION('ref_axis',(-1.,-2.22044604925031E-16,0.));
#3382=DIRECTION('center_axis',(2.22044604925031E-16,-1.,0.));
#3383=DIRECTION('ref_axis',(-1.,-2.22044604925031E-16,0.));
#3384=DIRECTION('center_axis',(-2.22044604925031E-16,1.,0.));
#3385=DIRECTION('ref_axis',(-1.,-2.22044604925031E-16,4.63931189975154E-15));
#3386=DIRECTION('center_axis',(-2.22044604925031E-16,1.,0.));
#3387=DIRECTION('ref_axis',(-1.,-2.22044604925031E-16,4.63931189975154E-15));
#3388=DIRECTION('center_axis',(-2.22044604925031E-16,1.,0.));
#3389=DIRECTION('ref_axis',(-1.,-2.22044604925031E-16,0.));
#3390=DIRECTION('',(-0.5,-1.11022302462516E-16,0.866025403784439));
#3391=DIRECTION('',(-1.,-2.22044604925031E-16,0.));
#3392=DIRECTION('',(-0.499999999999999,-1.11022302462515E-16,-0.866025403784439));
#3393=DIRECTION('',(0.5,1.11022302462516E-16,-0.866025403784438));
#3394=DIRECTION('',(1.,2.22044604925031E-16,4.80740671595891E-16));
#3395=DIRECTION('',(0.499999999999999,1.11022302462515E-16,0.866025403784439));
#3396=DIRECTION('center_axis',(0.866025403784439,1.92296268638356E-16,0.5));
#3397=DIRECTION('ref_axis',(-0.5,-1.11022302462516E-16,0.866025403784439));
#3398=DIRECTION('',(2.22044604925031E-16,-1.,0.));
#3399=DIRECTION('',(-0.5,-1.11022302462516E-16,0.866025403784439));
#3400=DIRECTION('',(2.22044604925031E-16,-1.,0.));
#3401=DIRECTION('center_axis',(0.866025403784439,1.92296268638356E-16,-0.499999999999999));
#3402=DIRECTION('ref_axis',(0.499999999999999,1.11022302462515E-16,0.866025403784439));
#3403=DIRECTION('',(2.22044604925031E-16,-1.,0.));
#3404=DIRECTION('',(0.499999999999999,1.11022302462515E-16,0.866025403784439));
#3405=DIRECTION('center_axis',(4.80740671595891E-16,1.06745872495904E-31,
-1.));
#3406=DIRECTION('ref_axis',(1.,2.22044604925031E-16,4.80740671595891E-16));
#3407=DIRECTION('',(2.22044604925031E-16,-1.,0.));
#3408=DIRECTION('',(1.,2.22044604925031E-16,4.80740671595891E-16));
#3409=DIRECTION('center_axis',(-0.866025403784438,-1.92296268638356E-16,
-0.5));
#3410=DIRECTION('ref_axis',(0.5,1.11022302462516E-16,-0.866025403784438));
#3411=DIRECTION('',(2.22044604925031E-16,-1.,0.));
#3412=DIRECTION('',(0.5,1.11022302462516E-16,-0.866025403784438));
#3413=DIRECTION('center_axis',(-0.866025403784439,-1.92296268638356E-16,
0.499999999999999));
#3414=DIRECTION('ref_axis',(-0.499999999999999,-1.11022302462515E-16,-0.866025403784439));
#3415=DIRECTION('',(2.22044604925031E-16,-1.,0.));
#3416=DIRECTION('',(-0.499999999999999,-1.11022302462515E-16,-0.866025403784439));
#3417=DIRECTION('center_axis',(0.,0.,1.));
#3418=DIRECTION('ref_axis',(-1.,-2.22044604925031E-16,0.));
#3419=DIRECTION('',(-1.,-2.22044604925031E-16,0.));
#3420=DIRECTION('center_axis',(2.22044604925031E-16,-1.,0.));
#3421=DIRECTION('ref_axis',(0.,0.,1.));
#3422=DIRECTION('center_axis',(-2.22044604925031E-16,1.,0.));
#3423=DIRECTION('ref_axis',(-1.,-2.22044604925031E-16,0.));
#3424=DIRECTION('',(0.,0.,1.));
#3425=DIRECTION('',(1.,0.,0.));
#3426=DIRECTION('',(0.,0.,1.));
#3427=DIRECTION('',(1.,0.,0.));
#3428=DIRECTION('',(0.,0.,1.));
#3429=DIRECTION('',(1.,0.,0.));
#3430=CARTESIAN_POINT('',(0.,0.,0.));
#3431=CARTESIAN_POINT('',(0.,0.,0.));
#3432=CARTESIAN_POINT('Origin',(0.,0.,3.64730359255819));
#3433=CARTESIAN_POINT('',(1.7686229373189,1.76804321859845,2.71234996365709));
#3434=CARTESIAN_POINT('',(-2.00054127207588,1.50061272066065,3.64730359255819));
#3435=CARTESIAN_POINT('Ctrl Pts',(1.76862293715133,1.76804321917473,2.7123499640497));
#3436=CARTESIAN_POINT('Ctrl Pts',(1.67326196575883,1.86343545816792,2.53195855620751));
#3437=CARTESIAN_POINT('Ctrl Pts',(1.55118349747322,1.96856998381331,2.36929449097458));
#3438=CARTESIAN_POINT('Ctrl Pts',(1.246000460916,2.17790854658287,2.06411145441735));
#3439=CARTESIAN_POINT('Ctrl Pts',(1.02949498881865,2.29363907921209,1.91141759608479));
#3440=CARTESIAN_POINT('Ctrl Pts',(0.539267048392588,2.45557152312544,1.70247672387608));
#3441=CARTESIAN_POINT('Ctrl Pts',(0.26499702638238,2.50080065552765,1.64676232048231));
#3442=CARTESIAN_POINT('Ctrl Pts',(-0.26499702638238,2.50080065552765,1.64676232048231));
#3443=CARTESIAN_POINT('Ctrl Pts',(-0.539267048392587,2.45557152312544,1.70247672387608));
#3444=CARTESIAN_POINT('Ctrl Pts',(-1.02949498881865,2.29363907921209,1.91141759608479));
#3445=CARTESIAN_POINT('Ctrl Pts',(-1.246000460916,2.17790854658287,2.06411145441735));
#3446=CARTESIAN_POINT('Ctrl Pts',(-1.58860233127999,1.94290274824875,2.40671332478134));
#3447=CARTESIAN_POINT('Ctrl Pts',(-1.73834101649832,1.80421211541924,2.62302156240085));
#3448=CARTESIAN_POINT('Ctrl Pts',(-1.89232803732295,1.6367193793479,2.98513719870131));
#3449=CARTESIAN_POINT('Ctrl Pts',(-1.93234128425375,1.58804832718918,3.11227541726051));
#3450=CARTESIAN_POINT('Ctrl Pts',(-1.98643480897785,1.51987885041677,3.37495601917005));
#3451=CARTESIAN_POINT('Ctrl Pts',(-2.00054127207588,1.50061272066065,3.51055323926873));
#3452=CARTESIAN_POINT('Ctrl Pts',(-2.00054127207588,1.50061272066065,3.64730359255819));
#3453=CARTESIAN_POINT('',(1.76857489436387,1.76809127600101,4.58234809718318));
#3454=CARTESIAN_POINT('Ctrl Pts',(1.76857489410945,1.76809127582596,4.5823480969561));
#3455=CARTESIAN_POINT('Ctrl Pts',(1.79165762592203,1.79117807736387,4.53868863499553));
#3456=CARTESIAN_POINT('Ctrl Pts',(1.81337315467134,1.81289707546748,4.49369536588909));
#3457=CARTESIAN_POINT('Ctrl Pts',(1.88690002208923,1.88643457058566,4.32522974835823));
#3458=CARTESIAN_POINT('Ctrl Pts',(1.92922149639063,1.92875988806683,4.19441050122833));
#3459=CARTESIAN_POINT('Ctrl Pts',(1.98603528459668,1.9855745276702,3.92446964748283));
#3460=CARTESIAN_POINT('Ctrl Pts',(2.00053500325065,2.00007126058529,3.78535115919203));
#3461=CARTESIAN_POINT('Ctrl Pts',(2.00054753639194,2.00007126058529,3.50944616688294));
#3462=CARTESIAN_POINT('Ctrl Pts',(1.98606217458304,1.98557625302193,3.37033412466248));
#3463=CARTESIAN_POINT('Ctrl Pts',(1.92927930620037,1.92876635631918,3.10040251938398));
#3464=CARTESIAN_POINT('Ctrl Pts',(1.88697439789821,1.88644406872771,2.96958607054619));
#3465=CARTESIAN_POINT('Ctrl Pts',(1.8134528306885,1.81289198848806,2.8010799828847));
#3466=CARTESIAN_POINT('Ctrl Pts',(1.79172259628398,1.79115269770373,2.7560468766317));
#3467=CARTESIAN_POINT('Ctrl Pts',(1.76862293706403,1.76804321842309,2.71234996388456));
#3468=CARTESIAN_POINT('Ctrl Pts',(-2.00054127207588,1.50061272066065,3.64730359255819));
#3469=CARTESIAN_POINT('Ctrl Pts',(-2.00054127207588,1.50061272066065,3.78405394584766));
#3470=CARTESIAN_POINT('Ctrl Pts',(-1.98643480897785,1.51987885041677,3.91965116594633));
#3471=CARTESIAN_POINT('Ctrl Pts',(-1.93234128425375,1.58804832718918,4.18233176785587));
#3472=CARTESIAN_POINT('Ctrl Pts',(-1.89232803732295,1.6367193793479,4.30946998641508));
#3473=CARTESIAN_POINT('Ctrl Pts',(-1.73834101649832,1.80421211541924,4.67158562271553));
#3474=CARTESIAN_POINT('Ctrl Pts',(-1.58860233127999,1.94290274824875,4.88789386033504));
#3475=CARTESIAN_POINT('Ctrl Pts',(-1.246000460916,2.17790854658287,5.23049573069903));
#3476=CARTESIAN_POINT('Ctrl Pts',(-1.02949498881865,2.29363907921209,5.38318958903159));
#3477=CARTESIAN_POINT('Ctrl Pts',(-0.539267048392588,2.45557152312544,5.5921304612403));
#3478=CARTESIAN_POINT('Ctrl Pts',(-0.26499702638238,2.50080065552765,5.64784486463407));
#3479=CARTESIAN_POINT('Ctrl Pts',(0.264997026382379,2.50080065552765,5.64784486463407));
#3480=CARTESIAN_POINT('Ctrl Pts',(0.539267048392587,2.45557152312544,5.5921304612403));
#3481=CARTESIAN_POINT('Ctrl Pts',(1.02949498881865,2.29363907921209,5.38318958903159));
#3482=CARTESIAN_POINT('Ctrl Pts',(1.246000460916,2.17790854658287,5.23049573069903));
#3483=CARTESIAN_POINT('Ctrl Pts',(1.55116056163378,1.96858571652152,4.92533562998125));
#3484=CARTESIAN_POINT('Ctrl Pts',(1.67322122242047,1.86347102998993,4.76270326620755));
#3485=CARTESIAN_POINT('Ctrl Pts',(1.76857489419661,1.76809127657624,4.58234809679125));
#3486=CARTESIAN_POINT('',(-2.00054127207588,6.65272805060642,3.64730359255819));
#3487=CARTESIAN_POINT('',(-2.00054127207588,0.,3.64730359255819));
#3488=CARTESIAN_POINT('',(2.00054127207588,6.65272805060642,3.64730359255819));
#3489=CARTESIAN_POINT('Ctrl Pts',(2.00054127207588,6.65272805060642,3.64730359255819));
#3490=CARTESIAN_POINT('Ctrl Pts',(2.00054127207588,6.65272805060642,3.90007910394674));
#3491=CARTESIAN_POINT('Ctrl Pts',(1.94972968142331,6.66864085099173,4.168651787778));
#3492=CARTESIAN_POINT('Ctrl Pts',(1.74514049605878,6.7250799896849,4.66107620583205));
#3493=CARTESIAN_POINT('Ctrl Pts',(1.59143342856617,6.76468178320297,4.88506276304886));
#3494=CARTESIAN_POINT('Ctrl Pts',(1.23780358335032,6.83823119596726,5.23869260826471));
#3495=CARTESIAN_POINT('Ctrl Pts',(1.01379886205209,6.87710358589666,5.39243413099089));
#3496=CARTESIAN_POINT('Ctrl Pts',(0.521308842207693,6.93185249060457,5.59704867604272));
#3497=CARTESIAN_POINT('Ctrl Pts',(0.25271202651198,6.94701057265674,5.64784486463407));
#3498=CARTESIAN_POINT('Ctrl Pts',(-0.25271202651198,6.94701057265674,5.64784486463407));
#3499=CARTESIAN_POINT('Ctrl Pts',(-0.521308842207694,6.93185249060457,5.59704867604272));
#3500=CARTESIAN_POINT('Ctrl Pts',(-1.01379886205209,6.87710358589666,5.39243413099088));
#3501=CARTESIAN_POINT('Ctrl Pts',(-1.23780358335032,6.83823119596726,5.23869260826471));
#3502=CARTESIAN_POINT('Ctrl Pts',(-1.59143342856617,6.76468178320297,4.88506276304886));
#3503=CARTESIAN_POINT('Ctrl Pts',(-1.74514049605878,6.7250799896849,4.66107620583205));
#3504=CARTESIAN_POINT('Ctrl Pts',(-1.94972968142331,6.66864085099173,4.168651787778));
#3505=CARTESIAN_POINT('Ctrl Pts',(-2.00054127207588,6.65272805060642,3.90007910394674));
#3506=CARTESIAN_POINT('Ctrl Pts',(-2.00054127207588,6.65272805060642,3.64730359255819));
#3507=CARTESIAN_POINT('Ctrl Pts',(-2.00054127207588,6.65272805060642,3.64730359255819));
#3508=CARTESIAN_POINT('Ctrl Pts',(-2.00054127207588,6.65272805060642,3.39452808116964));
#3509=CARTESIAN_POINT('Ctrl Pts',(-1.94972968142331,6.66864085099173,3.12595539733838));
#3510=CARTESIAN_POINT('Ctrl Pts',(-1.74514049605878,6.7250799896849,2.63353097928433));
#3511=CARTESIAN_POINT('Ctrl Pts',(-1.59143342856617,6.76468178320297,2.40954442206752));
#3512=CARTESIAN_POINT('Ctrl Pts',(-1.23780358335032,6.83823119596726,2.05591457685167));
#3513=CARTESIAN_POINT('Ctrl Pts',(-1.01379886205209,6.87710358589666,1.9021730541255));
#3514=CARTESIAN_POINT('Ctrl Pts',(-0.521308842207694,6.93185249060457,1.69755850907366));
#3515=CARTESIAN_POINT('Ctrl Pts',(-0.25271202651198,6.94701057265674,1.64676232048231));
#3516=CARTESIAN_POINT('Ctrl Pts',(0.25271202651198,6.94701057265674,1.64676232048231));
#3517=CARTESIAN_POINT('Ctrl Pts',(0.521308842207693,6.93185249060457,1.69755850907366));
#3518=CARTESIAN_POINT('Ctrl Pts',(1.01379886205209,6.87710358589666,1.9021730541255));
#3519=CARTESIAN_POINT('Ctrl Pts',(1.23780358335032,6.83823119596726,2.05591457685167));
#3520=CARTESIAN_POINT('Ctrl Pts',(1.59143342856617,6.76468178320297,2.40954442206752));
#3521=CARTESIAN_POINT('Ctrl Pts',(1.74514049605878,6.7250799896849,2.63353097928433));
#3522=CARTESIAN_POINT('Ctrl Pts',(1.94972968142331,6.66864085099173,3.12595539733838));
#3523=CARTESIAN_POINT('Ctrl Pts',(2.00054127207588,6.65272805060642,3.39452808116964));
#3524=CARTESIAN_POINT('Ctrl Pts',(2.00054127207588,6.65272805060642,3.64730359255819));
#3525=CARTESIAN_POINT('Origin',(0.,0.,7.74376865817678));
#3526=CARTESIAN_POINT('',(2.50080065552765,-3.06259751809754E-16,15.268401777045));
#3527=CARTESIAN_POINT('Origin',(0.,0.,15.268401777045));
#3528=CARTESIAN_POINT('',(2.50080065552765,-1.43519978267323E-17,5.64746572886916));
#3529=CARTESIAN_POINT('',(2.50080065552765,-3.06259751809754E-16,7.74376865817678));
#3530=CARTESIAN_POINT('',(1.50123911195662,-2.00007126058529,3.64739446828387));
#3531=CARTESIAN_POINT('Ctrl Pts',(2.50080065552765,2.77555756156289E-16,
5.64746572886916));
#3532=CARTESIAN_POINT('Ctrl Pts',(2.50080065552765,-0.264926868087175,5.64746572886916));
#3533=CARTESIAN_POINT('Ctrl Pts',(2.45559485322071,-0.539128651599931,5.59176763614851));
#3534=CARTESIAN_POINT('Ctrl Pts',(2.29374488883448,-1.02924237889175,5.38287897435064));
#3535=CARTESIAN_POINT('Ctrl Pts',(2.1780735274369,-1.24570166067483,5.23022071004141));
#3536=CARTESIAN_POINT('Ctrl Pts',(1.94320134506485,-1.58822705823722,4.88769531247902));
#3537=CARTESIAN_POINT('Ctrl Pts',(1.8045977690979,-1.73793406786513,4.67143479701259));
#3538=CARTESIAN_POINT('Ctrl Pts',(1.63722753567886,-1.89188688795684,4.30939601525252));
#3539=CARTESIAN_POINT('Ctrl Pts',(1.5885955233965,-1.93189082089362,4.18228427785571));
#3540=CARTESIAN_POINT('Ctrl Pts',(1.52048542524434,-1.98596995629194,3.91966465750307));
#3541=CARTESIAN_POINT('Ctrl Pts',(1.50123911195662,-2.00007126058529,3.78410209416443));
#3542=CARTESIAN_POINT('Ctrl Pts',(1.50123911195662,-2.00007126058529,3.64739446828387));
#3543=CARTESIAN_POINT('',(2.50080065552765,2.03424716928038E-17,1.64732320769858));
#3544=CARTESIAN_POINT('Ctrl Pts',(1.50123911195662,-2.00007126058529,3.64739446828387));
#3545=CARTESIAN_POINT('Ctrl Pts',(1.50123911195662,-2.00007126058529,3.51068684240331));
#3546=CARTESIAN_POINT('Ctrl Pts',(1.52048542524434,-1.98596995629194,3.37512427906467));
#3547=CARTESIAN_POINT('Ctrl Pts',(1.5885955233965,-1.93189082089362,3.11250465871203));
#3548=CARTESIAN_POINT('Ctrl Pts',(1.63722753567886,-1.89188688795684,2.98539292131522));
#3549=CARTESIAN_POINT('Ctrl Pts',(1.8045977690979,-1.73793406786513,2.62335413955515));
#3550=CARTESIAN_POINT('Ctrl Pts',(1.94320134506485,-1.58822705823722,2.40709362408872));
#3551=CARTESIAN_POINT('Ctrl Pts',(2.1780735274369,-1.24570166067483,2.06456822652633));
#3552=CARTESIAN_POINT('Ctrl Pts',(2.29374488883448,-1.02924237889175,1.9119099622171));
#3553=CARTESIAN_POINT('Ctrl Pts',(2.45559485322071,-0.53912865159993,1.70302130041923));
#3554=CARTESIAN_POINT('Ctrl Pts',(2.50080065552765,-0.264926868087175,1.64732320769858));
#3555=CARTESIAN_POINT('Ctrl Pts',(2.50080065552765,-1.38777878078145E-16,
1.64732320769858));
#3556=CARTESIAN_POINT('',(2.50080065552765,-3.06259751809754E-16,0.219135539308519));
#3557=CARTESIAN_POINT('',(2.50080065552765,-3.06259751809754E-16,7.74376865817678));
#3558=CARTESIAN_POINT('Origin',(0.,0.,0.219135539308519));
#3559=CARTESIAN_POINT('Ctrl Pts',(2.50080065552765,2.77555756156289E-16,
1.64732320769858));
#3560=CARTESIAN_POINT('Ctrl Pts',(2.50080065552765,0.264926868087175,1.64732320769858));
#3561=CARTESIAN_POINT('Ctrl Pts',(2.45559485322071,0.539128651599931,1.70302130041923));
#3562=CARTESIAN_POINT('Ctrl Pts',(2.29374488883448,1.02924237889175,1.9119099622171));
#3563=CARTESIAN_POINT('Ctrl Pts',(2.1780735274369,1.24570166067483,2.06456822652633));
#3564=CARTESIAN_POINT('Ctrl Pts',(1.96890768376227,1.55073826840574,2.36960483425724));
#3565=CARTESIAN_POINT('Ctrl Pts',(1.86390655010446,1.67272836391103,2.53212241175439));
#3566=CARTESIAN_POINT('Ctrl Pts',(1.76862293784399,1.76804321848184,2.71234996399565));
#3567=CARTESIAN_POINT('Ctrl Pts',(1.76857489488806,1.76809127588459,4.58234809684521));
#3568=CARTESIAN_POINT('Ctrl Pts',(1.863870991968,1.67276911284068,4.76261188718499));
#3569=CARTESIAN_POINT('Ctrl Pts',(1.96889195571996,1.55076120536613,4.92516116535011));
#3570=CARTESIAN_POINT('Ctrl Pts',(2.1780735274369,1.24570166067483,5.23022071004141));
#3571=CARTESIAN_POINT('Ctrl Pts',(2.29374488883448,1.02924237889175,5.38287897435064));
#3572=CARTESIAN_POINT('Ctrl Pts',(2.45559485322071,0.539128651599931,5.59176763614851));
#3573=CARTESIAN_POINT('Ctrl Pts',(2.50080065552765,0.264926868087175,5.64746572886916));
#3574=CARTESIAN_POINT('Ctrl Pts',(2.50080065552765,4.85722573273506E-16,
5.64746572886916));
#3575=CARTESIAN_POINT('Origin',(0.,0.,3.64739446828387));
#3576=CARTESIAN_POINT('',(6.65286936961679,-2.00007126058529,3.64739446828387));
#3577=CARTESIAN_POINT('',(0.,-2.00007126058529,3.64739446828387));
#3578=CARTESIAN_POINT('',(6.94701057265674,-5.29465121630953E-16,1.64732320769858));
#3579=CARTESIAN_POINT('Ctrl Pts',(6.94701057265674,-4.16333634234434E-16,
1.64732320769858));
#3580=CARTESIAN_POINT('Ctrl Pts',(6.94701057265674,-0.252651925025299,1.64732320769858));
#3581=CARTESIAN_POINT('Ctrl Pts',(6.93185967642424,-0.521185316397251,1.69810717591289));
#3582=CARTESIAN_POINT('Ctrl Pts',(6.87713670157391,-1.01355981516441,1.9026734267681));
#3583=CARTESIAN_POINT('Ctrl Pts',(6.83828274623297,-1.23751236388673,2.05637892973823));
#3584=CARTESIAN_POINT('Ctrl Pts',(6.76476847582112,-1.59105989763386,2.40992646348536));
#3585=CARTESIAN_POINT('Ctrl Pts',(6.7251858181423,-1.74473098673958,2.63386086947574));
#3586=CARTESIAN_POINT('Ctrl Pts',(6.66877424579284,-1.94927190878348,3.12616984589068));
#3587=CARTESIAN_POINT('Ctrl Pts',(6.65286936961679,-2.00007126058529,3.39467913557324));
#3588=CARTESIAN_POINT('Ctrl Pts',(6.65286936961679,-2.00007126058529,3.64739446828387));
#3589=CARTESIAN_POINT('',(6.94701057265674,-1.47825956916056E-16,5.64746572886916));
#3590=CARTESIAN_POINT('Ctrl Pts',(6.94701057265674,6.59194920871187E-16,
5.64746572886916));
#3591=CARTESIAN_POINT('Ctrl Pts',(6.94701057265674,0.252651925025299,5.64746572886916));
#3592=CARTESIAN_POINT('Ctrl Pts',(6.93185967642424,0.521185316397251,5.59668176065485));
#3593=CARTESIAN_POINT('Ctrl Pts',(6.87713670157391,1.01355981516441,5.39211550979964));
#3594=CARTESIAN_POINT('Ctrl Pts',(6.83828274623297,1.23751236388673,5.23841000682951));
#3595=CARTESIAN_POINT('Ctrl Pts',(6.76476847582112,1.59105989763386,4.88486247308238));
#3596=CARTESIAN_POINT('Ctrl Pts',(6.7251858181423,1.74473098673958,4.660928067092));
#3597=CARTESIAN_POINT('Ctrl Pts',(6.66877424579284,1.94927190878348,4.16861909067706));
#3598=CARTESIAN_POINT('Ctrl Pts',(6.65286936961679,2.00007126058529,3.9001098009945));
#3599=CARTESIAN_POINT('Ctrl Pts',(6.65286936961679,2.00007126058529,3.39467913557324));
#3600=CARTESIAN_POINT('Ctrl Pts',(6.66877424579284,1.94927190878348,3.12616984589068));
#3601=CARTESIAN_POINT('Ctrl Pts',(6.7251858181423,1.74473098673958,2.63386086947574));
#3602=CARTESIAN_POINT('Ctrl Pts',(6.76476847582112,1.59105989763386,2.40992646348536));
#3603=CARTESIAN_POINT('Ctrl Pts',(6.83828274623297,1.23751236388673,2.05637892973823));
#3604=CARTESIAN_POINT('Ctrl Pts',(6.87713670157391,1.01355981516441,1.9026734267681));
#3605=CARTESIAN_POINT('Ctrl Pts',(6.93185967642424,0.52118531639725,1.69810717591289));
#3606=CARTESIAN_POINT('Ctrl Pts',(6.94701057265674,0.252651925025298,1.64732320769858));
#3607=CARTESIAN_POINT('Ctrl Pts',(6.94701057265674,-4.16333634234434E-16,
1.64732320769858));
#3608=CARTESIAN_POINT('Ctrl Pts',(6.65286936961679,-2.00007126058529,3.64739446828387));
#3609=CARTESIAN_POINT('Ctrl Pts',(6.65286936961679,-2.00007126058529,3.9001098009945));
#3610=CARTESIAN_POINT('Ctrl Pts',(6.66877424579284,-1.94927190878348,4.16861909067706));
#3611=CARTESIAN_POINT('Ctrl Pts',(6.7251858181423,-1.74473098673957,4.660928067092));
#3612=CARTESIAN_POINT('Ctrl Pts',(6.76476847582112,-1.59105989763386,4.88486247308238));
#3613=CARTESIAN_POINT('Ctrl Pts',(6.83828274623297,-1.23751236388673,5.23841000682951));
#3614=CARTESIAN_POINT('Ctrl Pts',(6.87713670157391,-1.01355981516441,5.39211550979964));
#3615=CARTESIAN_POINT('Ctrl Pts',(6.93185967642424,-0.52118531639725,5.59668176065485));
#3616=CARTESIAN_POINT('Ctrl Pts',(6.94701057265674,-0.252651925025297,5.64746572886916));
#3617=CARTESIAN_POINT('Ctrl Pts',(6.94701057265674,8.32667268468867E-16,
5.64746572886916));
#3618=CARTESIAN_POINT('Origin',(4.58300560234995,1.11126133386797,7.30323111171487));
#3619=CARTESIAN_POINT('',(4.5963952096795,1.23456935960356,7.30323111171487));
#3620=CARTESIAN_POINT('',(4.5963952096795,1.23456935960356,14.3002311117149));
#3621=CARTESIAN_POINT('',(4.5963952096795,1.23456935960356,7.30323111171487));
#3622=CARTESIAN_POINT('',(4.5578337263362,1.23271308335391,7.30323111171487));
#3623=CARTESIAN_POINT('Origin',(4.58300560234995,1.11126133386797,7.30323111171487));
#3624=CARTESIAN_POINT('',(4.5578337263362,1.23271308335391,14.3002311117149));
#3625=CARTESIAN_POINT('',(4.5578337263362,1.23271308335391,7.30323111171487));
#3626=CARTESIAN_POINT('Origin',(4.58300560234995,1.11126133386797,14.3002311117149));
#3627=CARTESIAN_POINT('Origin',(4.69562204444668,2.09062562955478,14.3002311117149));
#3628=CARTESIAN_POINT('',(3.99305254500011,2.58969917173881,14.3002311117149));
#3629=CARTESIAN_POINT('Origin',(0.,0.,14.3002311117149));
#3630=CARTESIAN_POINT('',(3.96587039417894,2.562284496182,14.3002311117149));
#3631=CARTESIAN_POINT('Origin',(4.42403620092708,1.96970782149614,14.3002311117149));
#3632=CARTESIAN_POINT('Origin',(3.89245742766355,2.66225792836605,14.3002311117149));
#3633=CARTESIAN_POINT('Origin',(4.42403620092708,1.96970782149614,7.30323111171487));
#3634=CARTESIAN_POINT('',(3.96587039417894,2.562284496182,7.30323111171487));
#3635=CARTESIAN_POINT('Origin',(4.42403620092708,1.96970782149614,7.30323111171487));
#3636=CARTESIAN_POINT('',(3.96587039417894,2.562284496182,7.30323111171487));
#3637=CARTESIAN_POINT('Origin',(3.89245742766355,2.66225792836605,7.30323111171487));
#3638=CARTESIAN_POINT('',(3.99305254500011,2.58969917173881,7.30323111171487));
#3639=CARTESIAN_POINT('',(3.99305254500011,2.58969917173881,7.30323111171487));
#3640=CARTESIAN_POINT('Origin',(3.89245742766355,2.66225792836605,7.30323111171487));
#3641=CARTESIAN_POINT('Origin',(3.73479324586,2.87926405770635,7.30323111171487));
#3642=CARTESIAN_POINT('',(3.69687136836352,2.99735758844529,7.30323111171487));
#3643=CARTESIAN_POINT('',(3.69687136836352,2.99735758844529,14.3002311117149));
#3644=CARTESIAN_POINT('',(3.69687136836352,2.99735758844529,7.30323111171487));
#3645=CARTESIAN_POINT('',(3.6623987159857,2.97997742742222,7.30323111171487));
#3646=CARTESIAN_POINT('Origin',(3.73479324586,2.87926405770635,7.30323111171487));
#3647=CARTESIAN_POINT('',(3.6623987159857,2.97997742742222,14.3002311117149));
#3648=CARTESIAN_POINT('',(3.6623987159857,2.97997742742222,7.30323111171487));
#3649=CARTESIAN_POINT('Origin',(3.73479324586,2.87926405770635,14.3002311117149));
#3650=CARTESIAN_POINT('Origin',(3.43933013901738,3.81976309502194,14.3002311117149));
#3651=CARTESIAN_POINT('',(2.59450946692386,3.98992870278142,14.3002311117149));
#3652=CARTESIAN_POINT('Origin',(0.,0.,14.3002311117149));
#3653=CARTESIAN_POINT('',(2.5808278896192,3.95382817367717,14.3002311117149));
#3654=CARTESIAN_POINT('Origin',(3.24040582864787,3.59883526642179,14.3002311117149));
#3655=CARTESIAN_POINT('Origin',(2.4730989493237,4.01529870497514,14.3002311117149));
#3656=CARTESIAN_POINT('Origin',(3.24040582864787,3.59883526642179,7.30323111171487));
#3657=CARTESIAN_POINT('',(2.5808278896192,3.95382817367717,7.30323111171487));
#3658=CARTESIAN_POINT('Origin',(3.24040582864787,3.59883526642179,7.30323111171487));
#3659=CARTESIAN_POINT('',(2.5808278896192,3.95382817367717,7.30323111171487));
#3660=CARTESIAN_POINT('Origin',(2.4730989493237,4.01529870497514,7.30323111171487));
#3661=CARTESIAN_POINT('',(2.59450946692386,3.98992870278142,7.30323111171487));
#3662=CARTESIAN_POINT('',(2.59450946692386,3.98992870278142,7.30323111171487));
#3663=CARTESIAN_POINT('Origin',(2.4730989493237,4.01529870497514,7.30323111171487));
#3664=CARTESIAN_POINT('Origin',(2.24080120762938,4.1494158686745,7.30323111171487));
#3665=CARTESIAN_POINT('',(2.15812488243547,4.241875460106,7.30323111171487));
#3666=CARTESIAN_POINT('',(2.15812488243547,4.241875460106,14.3002311117149));
#3667=CARTESIAN_POINT('',(2.15812488243547,4.241875460106,7.30323111171487));
#3668=CARTESIAN_POINT('',(2.13370169579345,4.2119766020442,7.30323111171487));
#3669=CARTESIAN_POINT('Origin',(2.24080120762938,4.1494158686745,7.30323111171487));
#3670=CARTESIAN_POINT('',(2.13370169579345,4.2119766020442,14.3002311117149));
#3671=CARTESIAN_POINT('',(2.13370169579345,4.2119766020442,7.30323111171487));
#3672=CARTESIAN_POINT('Origin',(2.24080120762938,4.1494158686745,14.3002311117149));
#3673=CARTESIAN_POINT('Origin',(1.58834680721857,4.88842881990149,14.3002311117149));
#3674=CARTESIAN_POINT('',(0.74735213163792,4.7002633137488,14.3002311117149));
#3675=CARTESIAN_POINT('Origin',(0.,0.,14.3002311117149));
#3676=CARTESIAN_POINT('',(0.749536796858992,4.66171904054223,14.3002311117149));
#3677=CARTESIAN_POINT('Origin',(1.49647985043267,4.60569139939112,14.3002311117149));
#3678=CARTESIAN_POINT('Origin',(0.62611919524716,4.67405785765047,14.3002311117149));
#3679=CARTESIAN_POINT('Origin',(1.49647985043267,4.60569139939112,7.30323111171487));
#3680=CARTESIAN_POINT('',(0.749536796858992,4.66171904054223,7.30323111171487));
#3681=CARTESIAN_POINT('Origin',(1.49647985043267,4.60569139939112,7.30323111171487));
#3682=CARTESIAN_POINT('',(0.749536796858992,4.66171904054223,7.30323111171487));
#3683=CARTESIAN_POINT('Origin',(0.62611919524716,4.67405785765047,7.30323111171487));
#3684=CARTESIAN_POINT('',(0.74735213163792,4.7002633137488,7.30323111171487));
#3685=CARTESIAN_POINT('',(0.74735213163792,4.7002633137488,7.30323111171487));
#3686=CARTESIAN_POINT('Origin',(0.62611919524716,4.67405785765047,7.30323111171487));
#3687=CARTESIAN_POINT('Origin',(0.359354283559748,4.70209597968909,7.30323111171487));
#3688=CARTESIAN_POINT('',(0.246218998385265,4.75293452848561,7.30323111171487));
#3689=CARTESIAN_POINT('',(0.246218998385265,4.75293452848561,14.3002311117149));
#3690=CARTESIAN_POINT('',(0.246218998385265,4.75293452848561,7.30323111171487));
#3691=CARTESIAN_POINT('',(0.236068268327149,4.71568675756656,7.30323111171487));
#3692=CARTESIAN_POINT('Origin',(0.359354283559748,4.70209597968909,7.30323111171487));
#3693=CARTESIAN_POINT('',(0.236068268327149,4.71568675756656,14.3002311117149));
#3694=CARTESIAN_POINT('',(0.236068268327149,4.71568675756656,7.30323111171487));
#3695=CARTESIAN_POINT('Origin',(0.359354283559748,4.70209597968909,14.3002311117149));
#3696=CARTESIAN_POINT('Origin',(-0.537276117226072,5.11184079183843,14.3002311117149));
#3697=CARTESIAN_POINT('',(-1.22902917668919,4.59787969721732,14.3002311117149));
#3698=CARTESIAN_POINT('Origin',(0.,0.,14.3002311117149));
#3699=CARTESIAN_POINT('',(-1.21135601740617,4.5635563349096,14.3002311117149));
#3700=CARTESIAN_POINT('Origin',(-0.506201089014987,4.81618164801291,14.3002311117149));
#3701=CARTESIAN_POINT('Origin',(-1.32912225580194,4.52462994425545,14.3002311117149));
#3702=CARTESIAN_POINT('Origin',(-0.506201089014987,4.81618164801291,7.30323111171487));
#3703=CARTESIAN_POINT('',(-1.21135601740617,4.5635563349096,7.30323111171487));
#3704=CARTESIAN_POINT('Origin',(-0.506201089014987,4.81618164801291,7.30323111171487));
#3705=CARTESIAN_POINT('',(-1.21135601740617,4.5635563349096,7.30323111171487));
#3706=CARTESIAN_POINT('Origin',(-1.32912225580194,4.52462994425545,7.30323111171487));
#3707=CARTESIAN_POINT('',(-1.22902917668919,4.59787969721732,7.30323111171487));
#3708=CARTESIAN_POINT('',(-1.22902917668919,4.59787969721732,7.30323111171487));
#3709=CARTESIAN_POINT('Origin',(-1.32912225580194,4.52462994425545,7.30323111171487));
#3710=CARTESIAN_POINT('Origin',(-1.58422826076854,4.44174097861451,7.30323111171487));
#3711=CARTESIAN_POINT('',(-1.70826038731513,4.44216803783541,7.30323111171487));
#3712=CARTESIAN_POINT('',(-1.70826038731513,4.44216803783541,14.3002311117149));
#3713=CARTESIAN_POINT('',(-1.70826038731513,4.44216803783541,7.30323111171487));
#3714=CARTESIAN_POINT('',(-1.70238350734581,4.4040118320364,7.30323111171487));
#3715=CARTESIAN_POINT('Origin',(-1.58422826076854,4.44174097861451,7.30323111171487));
#3716=CARTESIAN_POINT('',(-1.70238350734581,4.4040118320364,14.3002311117149));
#3717=CARTESIAN_POINT('',(-1.70238350734581,4.4040118320364,7.30323111171487));
#3718=CARTESIAN_POINT('Origin',(-1.58422826076854,4.44174097861451,14.3002311117149));
#3719=CARTESIAN_POINT('Origin',(-2.56999912000204,4.45136905125082,14.3002311117149));
#3720=CARTESIAN_POINT('',(-2.99290017498718,3.70048091061125,14.3002311117149));
#3721=CARTESIAN_POINT('Origin',(0.,0.,14.3002311117149));
#3722=CARTESIAN_POINT('',(-2.96279437143787,3.67631328036332,14.3002311117149));
#3723=CARTESIAN_POINT('Origin',(-2.42135526147943,4.19391033605658,14.3002311117149));
#3724=CARTESIAN_POINT('Origin',(-3.05454639412625,3.59285240852604,14.3002311117149));
#3725=CARTESIAN_POINT('Origin',(-2.42135526147943,4.19391033605658,7.30323111171487));
#3726=CARTESIAN_POINT('',(-2.96279437143787,3.67631328036332,7.30323111171487));
#3727=CARTESIAN_POINT('Origin',(-2.42135526147943,4.19391033605658,7.30323111171487));
#3728=CARTESIAN_POINT('',(-2.96279437143787,3.67631328036332,7.30323111171487));
#3729=CARTESIAN_POINT('Origin',(-3.05454639412625,3.59285240852604,7.30323111171487));
#3730=CARTESIAN_POINT('',(-2.99290017498718,3.70048091061125,7.30323111171487));
#3731=CARTESIAN_POINT('',(-2.99290017498718,3.70048091061125,7.30323111171487));
#3732=CARTESIAN_POINT('Origin',(-3.05454639412625,3.59285240852604,7.30323111171487));
#3733=CARTESIAN_POINT('Origin',(-3.25388334654802,3.41336861038748,7.30323111171487));
#3734=CARTESIAN_POINT('',(-3.36736603299031,3.36331033761377,7.30323111171487));
#3735=CARTESIAN_POINT('',(-3.36736603299031,3.36331033761377,14.3002311117149));
#3736=CARTESIAN_POINT('',(-3.36736603299031,3.36331033761377,7.30323111171487));
#3737=CARTESIAN_POINT('',(-3.34647770893003,3.33084325155569,7.30323111171487));
#3738=CARTESIAN_POINT('Origin',(-3.25388334654802,3.41336861038748,7.30323111171487));
#3739=CARTESIAN_POINT('',(-3.34647770893003,3.33084325155569,14.3002311117149));
#3740=CARTESIAN_POINT('',(-3.34647770893003,3.33084325155569,7.30323111171487));
#3741=CARTESIAN_POINT('Origin',(-3.25388334654802,3.41336861038748,14.3002311117149));
#3742=CARTESIAN_POINT('Origin',(-4.15834592722061,3.02121516228366,14.3002311117149));
#3743=CARTESIAN_POINT('',(-4.23927154338538,2.1632353567468,14.3002311117149));
#3744=CARTESIAN_POINT('Origin',(0.,0.,14.3002311117149));
#3745=CARTESIAN_POINT('',(-4.20193866250609,2.15340226138457,14.3002311117149));
#3746=CARTESIAN_POINT('Origin',(-3.9178351119121,2.84647382651678,14.3002311117149));
#3747=CARTESIAN_POINT('Origin',(-4.25181171122331,2.03983805132304,14.3002311117149));
#3748=CARTESIAN_POINT('Origin',(-3.9178351119121,2.84647382651678,7.30323111171487));
#3749=CARTESIAN_POINT('',(-4.20193866250609,2.15340226138457,7.30323111171487));
#3750=CARTESIAN_POINT('Origin',(-3.9178351119121,2.84647382651678,7.30323111171487));
#3751=CARTESIAN_POINT('',(-4.20193866250609,2.15340226138457,7.30323111171487));
#3752=CARTESIAN_POINT('Origin',(-4.25181171122331,2.03983805132304,7.30323111171487));
#3753=CARTESIAN_POINT('',(-4.23927154338538,2.1632353567468,7.30323111171487));
#3754=CARTESIAN_POINT('',(-4.23927154338538,2.1632353567468,7.30323111171487));
#3755=CARTESIAN_POINT('Origin',(-4.25181171122331,2.03983805132304,7.30323111171487));
#3756=CARTESIAN_POINT('Origin',(-4.36091244110716,1.79479379994412,7.30323111171487));
#3757=CARTESIAN_POINT('',(-4.44422350000145,1.70290572530351,7.30323111171487));
#3758=CARTESIAN_POINT('',(-4.44422350000145,1.70290572530351,14.3002311117149));
#3759=CARTESIAN_POINT('',(-4.44422350000145,1.70290572530351,7.30323111171487));
#3760=CARTESIAN_POINT('',(-4.41193551284469,1.68174161312001,7.30323111171487));
#3761=CARTESIAN_POINT('Origin',(-4.36091244110716,1.79479379994412,7.30323111171487));
#3762=CARTESIAN_POINT('',(-4.41193551284469,1.68174161312001,14.3002311117149));
#3763=CARTESIAN_POINT('',(-4.41193551284469,1.68174161312001,7.30323111171487));
#3764=CARTESIAN_POINT('Origin',(-4.36091244110716,1.79479379994412,14.3002311117149));
#3765=CARTESIAN_POINT('Origin',(-5.02767694623596,1.06866572487955,14.3002311117149));
#3766=CARTESIAN_POINT('',(-4.75263434935933,0.251946757324573,14.3002311117149));
#3767=CARTESIAN_POINT('Origin',(0.,0.,14.3002311117149));
#3768=CARTESIAN_POINT('',(-4.71452958541266,0.258148428367029,14.3002311117149));
#3769=CARTESIAN_POINT('Origin',(-4.73688567908055,1.00685613296933,14.3002311117149));
#3770=CARTESIAN_POINT('Origin',(-4.71390015695308,0.134117163699359,14.3002311117149));
#3771=CARTESIAN_POINT('Origin',(-4.73688567908055,1.00685613296933,7.30323111171487));
#3772=CARTESIAN_POINT('',(-4.71452958541266,0.258148428367029,7.30323111171487));
#3773=CARTESIAN_POINT('Origin',(-4.73688567908055,1.00685613296933,7.30323111171487));
#3774=CARTESIAN_POINT('',(-4.71452958541266,0.258148428367029,7.30323111171487));
#3775=CARTESIAN_POINT('Origin',(-4.71390015695308,0.134117163699359,7.30323111171487));
#3776=CARTESIAN_POINT('',(-4.75263434935933,0.251946757324573,7.30323111171487));
#3777=CARTESIAN_POINT('',(-4.75263434935933,0.251946757324573,7.30323111171487));
#3778=CARTESIAN_POINT('Origin',(-4.71390015695308,0.134117163699359,7.30323111171487));
#3779=CARTESIAN_POINT('Origin',(-4.71390015695308,-0.134117163699362,7.30323111171487));
#3780=CARTESIAN_POINT('',(-4.75263434935933,-0.251946757324576,7.30323111171487));
#3781=CARTESIAN_POINT('',(-4.75263434935933,-0.251946757324576,14.3002311117149));
#3782=CARTESIAN_POINT('',(-4.75263434935933,-0.251946757324576,7.30323111171487));
#3783=CARTESIAN_POINT('',(-4.71452958541266,-0.258148428367032,7.30323111171487));
#3784=CARTESIAN_POINT('Origin',(-4.71390015695308,-0.134117163699362,7.30323111171487));
#3785=CARTESIAN_POINT('',(-4.71452958541266,-0.258148428367032,14.3002311117149));
#3786=CARTESIAN_POINT('',(-4.71452958541266,-0.258148428367032,7.30323111171487));
#3787=CARTESIAN_POINT('Origin',(-4.71390015695308,-0.134117163699362,14.3002311117149));
#3788=CARTESIAN_POINT('Origin',(-5.02767694623596,-1.06866572487955,14.3002311117149));
#3789=CARTESIAN_POINT('',(-4.44422350000145,-1.70290572530351,14.3002311117149));
#3790=CARTESIAN_POINT('Origin',(0.,0.,14.3002311117149));
#3791=CARTESIAN_POINT('',(-4.41193551284469,-1.68174161312001,14.3002311117149));
#3792=CARTESIAN_POINT('Origin',(-4.73688567908055,-1.00685613296933,14.3002311117149));
#3793=CARTESIAN_POINT('Origin',(-4.36091244110716,-1.79479379994413,14.3002311117149));
#3794=CARTESIAN_POINT('Origin',(-4.73688567908055,-1.00685613296933,7.30323111171487));
#3795=CARTESIAN_POINT('',(-4.41193551284469,-1.68174161312001,7.30323111171487));
#3796=CARTESIAN_POINT('Origin',(-4.73688567908055,-1.00685613296933,7.30323111171487));
#3797=CARTESIAN_POINT('',(-4.41193551284469,-1.68174161312001,7.30323111171487));
#3798=CARTESIAN_POINT('Origin',(-4.36091244110716,-1.79479379994413,7.30323111171487));
#3799=CARTESIAN_POINT('',(-4.44422350000145,-1.70290572530351,7.30323111171487));
#3800=CARTESIAN_POINT('',(-4.44422350000145,-1.70290572530351,7.30323111171487));
#3801=CARTESIAN_POINT('Origin',(-4.36091244110716,-1.79479379994413,7.30323111171487));
#3802=CARTESIAN_POINT('Origin',(-4.25181171122331,-2.03983805132304,7.30323111171487));
#3803=CARTESIAN_POINT('',(-4.23927154338538,-2.1632353567468,7.30323111171487));
#3804=CARTESIAN_POINT('',(-4.23927154338538,-2.1632353567468,14.3002311117149));
#3805=CARTESIAN_POINT('',(-4.23927154338538,-2.1632353567468,7.30323111171487));
#3806=CARTESIAN_POINT('',(-4.20193866250609,-2.15340226138457,7.30323111171487));
#3807=CARTESIAN_POINT('Origin',(-4.25181171122331,-2.03983805132304,7.30323111171487));
#3808=CARTESIAN_POINT('',(-4.20193866250609,-2.15340226138457,14.3002311117149));
#3809=CARTESIAN_POINT('',(-4.20193866250609,-2.15340226138457,7.30323111171487));
#3810=CARTESIAN_POINT('Origin',(-4.25181171122331,-2.03983805132304,14.3002311117149));
#3811=CARTESIAN_POINT('Origin',(-4.15834592722061,-3.02121516228366,14.3002311117149));
#3812=CARTESIAN_POINT('',(-3.36736603299031,-3.36331033761377,14.3002311117149));
#3813=CARTESIAN_POINT('Origin',(0.,0.,14.3002311117149));
#3814=CARTESIAN_POINT('',(-3.34647770893003,-3.33084325155569,14.3002311117149));
#3815=CARTESIAN_POINT('Origin',(-3.91783511191209,-2.84647382651678,14.3002311117149));
#3816=CARTESIAN_POINT('Origin',(-3.25388334654802,-3.41336861038748,14.3002311117149));
#3817=CARTESIAN_POINT('Origin',(-3.91783511191209,-2.84647382651678,7.30323111171487));
#3818=CARTESIAN_POINT('',(-3.34647770893003,-3.33084325155569,7.30323111171487));
#3819=CARTESIAN_POINT('Origin',(-3.91783511191209,-2.84647382651678,7.30323111171487));
#3820=CARTESIAN_POINT('',(-3.34647770893003,-3.33084325155569,7.30323111171487));
#3821=CARTESIAN_POINT('Origin',(-3.25388334654802,-3.41336861038748,7.30323111171487));
#3822=CARTESIAN_POINT('',(-3.36736603299031,-3.36331033761377,7.30323111171487));
#3823=CARTESIAN_POINT('',(-3.36736603299031,-3.36331033761377,7.30323111171487));
#3824=CARTESIAN_POINT('Origin',(-3.25388334654802,-3.41336861038748,7.30323111171487));
#3825=CARTESIAN_POINT('Origin',(-3.05454639412625,-3.59285240852604,7.30323111171487));
#3826=CARTESIAN_POINT('',(-2.99290017498718,-3.70048091061125,7.30323111171487));
#3827=CARTESIAN_POINT('',(-2.99290017498718,-3.70048091061125,14.3002311117149));
#3828=CARTESIAN_POINT('',(-2.99290017498718,-3.70048091061125,7.30323111171487));
#3829=CARTESIAN_POINT('',(-2.96279437143787,-3.67631328036332,7.30323111171487));
#3830=CARTESIAN_POINT('Origin',(-3.05454639412625,-3.59285240852604,7.30323111171487));
#3831=CARTESIAN_POINT('',(-2.96279437143787,-3.67631328036332,14.3002311117149));
#3832=CARTESIAN_POINT('',(-2.96279437143787,-3.67631328036332,7.30323111171487));
#3833=CARTESIAN_POINT('Origin',(-3.05454639412625,-3.59285240852604,14.3002311117149));
#3834=CARTESIAN_POINT('Origin',(-2.56999912000203,-4.45136905125083,14.3002311117149));
#3835=CARTESIAN_POINT('',(-1.70826038731512,-4.44216803783542,14.3002311117149));
#3836=CARTESIAN_POINT('Origin',(0.,0.,14.3002311117149));
#3837=CARTESIAN_POINT('',(-1.7023835073458,-4.4040118320364,14.3002311117149));
#3838=CARTESIAN_POINT('Origin',(-2.42135526147942,-4.19391033605659,14.3002311117149));
#3839=CARTESIAN_POINT('Origin',(-1.58422826076853,-4.44174097861451,14.3002311117149));
#3840=CARTESIAN_POINT('Origin',(-2.42135526147942,-4.19391033605659,7.30323111171487));
#3841=CARTESIAN_POINT('',(-1.7023835073458,-4.4040118320364,7.30323111171487));
#3842=CARTESIAN_POINT('Origin',(-2.42135526147942,-4.19391033605659,7.30323111171487));
#3843=CARTESIAN_POINT('',(-1.7023835073458,-4.4040118320364,7.30323111171487));
#3844=CARTESIAN_POINT('Origin',(-1.58422826076853,-4.44174097861451,7.30323111171487));
#3845=CARTESIAN_POINT('',(-1.70826038731512,-4.44216803783542,7.30323111171487));
#3846=CARTESIAN_POINT('',(-1.70826038731512,-4.44216803783542,7.30323111171487));
#3847=CARTESIAN_POINT('Origin',(-1.58422826076853,-4.44174097861451,7.30323111171487));
#3848=CARTESIAN_POINT('Origin',(-1.32912225580193,-4.52462994425545,7.30323111171487));
#3849=CARTESIAN_POINT('',(-1.22902917668918,-4.59787969721732,7.30323111171487));
#3850=CARTESIAN_POINT('',(-1.22902917668918,-4.59787969721732,14.3002311117149));
#3851=CARTESIAN_POINT('',(-1.22902917668918,-4.59787969721732,7.30323111171487));
#3852=CARTESIAN_POINT('',(-1.21135601740617,-4.5635563349096,7.30323111171487));
#3853=CARTESIAN_POINT('Origin',(-1.32912225580193,-4.52462994425545,7.30323111171487));
#3854=CARTESIAN_POINT('',(-1.21135601740617,-4.5635563349096,14.3002311117149));
#3855=CARTESIAN_POINT('',(-1.21135601740617,-4.5635563349096,7.30323111171487));
#3856=CARTESIAN_POINT('Origin',(-1.32912225580193,-4.52462994425545,14.3002311117149));
#3857=CARTESIAN_POINT('Origin',(-0.537276117226068,-5.11184079183843,14.3002311117149));
#3858=CARTESIAN_POINT('',(0.246218998385269,-4.75293452848561,14.3002311117149));
#3859=CARTESIAN_POINT('Origin',(0.,0.,14.3002311117149));
#3860=CARTESIAN_POINT('',(0.236068268327154,-4.71568675756656,14.3002311117149));
#3861=CARTESIAN_POINT('Origin',(-0.506201089014981,-4.81618164801291,14.3002311117149));
#3862=CARTESIAN_POINT('Origin',(0.359354283559752,-4.70209597968909,14.3002311117149));
#3863=CARTESIAN_POINT('Origin',(-0.506201089014981,-4.81618164801291,7.30323111171487));
#3864=CARTESIAN_POINT('',(0.236068268327154,-4.71568675756656,7.30323111171487));
#3865=CARTESIAN_POINT('Origin',(-0.506201089014981,-4.81618164801291,7.30323111171487));
#3866=CARTESIAN_POINT('',(0.236068268327154,-4.71568675756656,7.30323111171487));
#3867=CARTESIAN_POINT('Origin',(0.359354283559752,-4.70209597968909,7.30323111171487));
#3868=CARTESIAN_POINT('',(0.246218998385269,-4.75293452848561,7.30323111171487));
#3869=CARTESIAN_POINT('',(0.246218998385269,-4.75293452848561,7.30323111171487));
#3870=CARTESIAN_POINT('Origin',(0.359354283559752,-4.70209597968909,7.30323111171487));
#3871=CARTESIAN_POINT('Origin',(0.626119195247162,-4.67405785765047,7.30323111171487));
#3872=CARTESIAN_POINT('',(0.747352131637922,-4.7002633137488,7.30323111171487));
#3873=CARTESIAN_POINT('',(0.747352131637922,-4.7002633137488,14.3002311117149));
#3874=CARTESIAN_POINT('',(0.747352131637922,-4.7002633137488,7.30323111171487));
#3875=CARTESIAN_POINT('',(0.749536796858993,-4.66171904054223,7.30323111171487));
#3876=CARTESIAN_POINT('Origin',(0.626119195247162,-4.67405785765047,7.30323111171487));
#3877=CARTESIAN_POINT('',(0.749536796858993,-4.66171904054223,14.3002311117149));
#3878=CARTESIAN_POINT('',(0.749536796858993,-4.66171904054223,7.30323111171487));
#3879=CARTESIAN_POINT('Origin',(0.626119195247162,-4.67405785765047,14.3002311117149));
#3880=CARTESIAN_POINT('Origin',(1.58834680721858,-4.88842881990149,14.3002311117149));
#3881=CARTESIAN_POINT('',(2.15812488243547,-4.24187546010599,14.3002311117149));
#3882=CARTESIAN_POINT('Origin',(0.,0.,14.3002311117149));
#3883=CARTESIAN_POINT('',(2.13370169579346,-4.2119766020442,14.3002311117149));
#3884=CARTESIAN_POINT('Origin',(1.49647985043267,-4.60569139939112,14.3002311117149));
#3885=CARTESIAN_POINT('Origin',(2.24080120762938,-4.1494158686745,14.3002311117149));
#3886=CARTESIAN_POINT('Origin',(1.49647985043267,-4.60569139939112,7.30323111171487));
#3887=CARTESIAN_POINT('',(2.13370169579346,-4.2119766020442,7.30323111171487));
#3888=CARTESIAN_POINT('Origin',(1.49647985043267,-4.60569139939112,7.30323111171487));
#3889=CARTESIAN_POINT('',(2.13370169579346,-4.2119766020442,7.30323111171487));
#3890=CARTESIAN_POINT('Origin',(2.24080120762938,-4.1494158686745,7.30323111171487));
#3891=CARTESIAN_POINT('',(2.15812488243547,-4.24187546010599,7.30323111171487));
#3892=CARTESIAN_POINT('',(2.15812488243547,-4.24187546010599,7.30323111171487));
#3893=CARTESIAN_POINT('Origin',(2.24080120762938,-4.1494158686745,7.30323111171487));
#3894=CARTESIAN_POINT('Origin',(2.4730989493237,-4.01529870497514,7.30323111171487));
#3895=CARTESIAN_POINT('',(2.59450946692386,-3.98992870278142,7.30323111171487));
#3896=CARTESIAN_POINT('',(2.59450946692386,-3.98992870278142,14.3002311117149));
#3897=CARTESIAN_POINT('',(2.59450946692386,-3.98992870278142,7.30323111171487));
#3898=CARTESIAN_POINT('',(2.58082788961921,-3.95382817367717,7.30323111171487));
#3899=CARTESIAN_POINT('Origin',(2.4730989493237,-4.01529870497514,7.30323111171487));
#3900=CARTESIAN_POINT('',(2.58082788961921,-3.95382817367717,14.3002311117149));
#3901=CARTESIAN_POINT('',(2.58082788961921,-3.95382817367717,7.30323111171487));
#3902=CARTESIAN_POINT('Origin',(2.4730989493237,-4.01529870497514,14.3002311117149));
#3903=CARTESIAN_POINT('Origin',(3.43933013901739,-3.81976309502194,14.3002311117149));
#3904=CARTESIAN_POINT('',(3.69687136836353,-2.99735758844529,14.3002311117149));
#3905=CARTESIAN_POINT('Origin',(0.,0.,14.3002311117149));
#3906=CARTESIAN_POINT('',(3.6623987159857,-2.97997742742222,14.3002311117149));
#3907=CARTESIAN_POINT('Origin',(3.24040582864788,-3.59883526642179,14.3002311117149));
#3908=CARTESIAN_POINT('Origin',(3.73479324586,-2.87926405770635,14.3002311117149));
#3909=CARTESIAN_POINT('Origin',(3.24040582864788,-3.59883526642179,7.30323111171487));
#3910=CARTESIAN_POINT('',(3.6623987159857,-2.97997742742222,7.30323111171487));
#3911=CARTESIAN_POINT('Origin',(3.24040582864788,-3.59883526642179,7.30323111171487));
#3912=CARTESIAN_POINT('',(3.6623987159857,-2.97997742742222,7.30323111171487));
#3913=CARTESIAN_POINT('Origin',(3.73479324586,-2.87926405770635,7.30323111171487));
#3914=CARTESIAN_POINT('',(3.69687136836353,-2.99735758844529,7.30323111171487));
#3915=CARTESIAN_POINT('',(3.69687136836353,-2.99735758844529,7.30323111171487));
#3916=CARTESIAN_POINT('Origin',(3.73479324586,-2.87926405770635,7.30323111171487));
#3917=CARTESIAN_POINT('Origin',(3.89245742766356,-2.66225792836605,7.30323111171487));
#3918=CARTESIAN_POINT('',(3.99305254500012,-2.58969917173881,7.30323111171487));
#3919=CARTESIAN_POINT('',(3.99305254500012,-2.58969917173881,14.3002311117149));
#3920=CARTESIAN_POINT('',(3.99305254500012,-2.58969917173881,7.30323111171487));
#3921=CARTESIAN_POINT('',(3.96587039417894,-2.562284496182,7.30323111171487));
#3922=CARTESIAN_POINT('Origin',(3.89245742766356,-2.66225792836605,7.30323111171487));
#3923=CARTESIAN_POINT('',(3.96587039417894,-2.562284496182,14.3002311117149));
#3924=CARTESIAN_POINT('',(3.96587039417894,-2.562284496182,7.30323111171487));
#3925=CARTESIAN_POINT('Origin',(3.89245742766356,-2.66225792836605,14.3002311117149));
#3926=CARTESIAN_POINT('Origin',(4.69562204444668,-2.09062562955477,14.3002311117149));
#3927=CARTESIAN_POINT('',(4.5963952096795,-1.23456935960355,14.3002311117149));
#3928=CARTESIAN_POINT('Origin',(0.,0.,14.3002311117149));
#3929=CARTESIAN_POINT('',(4.5578337263362,-1.23271308335391,14.3002311117149));
#3930=CARTESIAN_POINT('Origin',(4.42403620092708,-1.96970782149613,14.3002311117149));
#3931=CARTESIAN_POINT('Origin',(4.58300560234995,-1.11126133386797,14.3002311117149));
#3932=CARTESIAN_POINT('Origin',(4.42403620092708,-1.96970782149613,7.30323111171487));
#3933=CARTESIAN_POINT('',(4.5578337263362,-1.23271308335391,7.30323111171487));
#3934=CARTESIAN_POINT('Origin',(4.42403620092708,-1.96970782149613,7.30323111171487));
#3935=CARTESIAN_POINT('',(4.5578337263362,-1.23271308335391,7.30323111171487));
#3936=CARTESIAN_POINT('Origin',(4.58300560234995,-1.11126133386797,7.30323111171487));
#3937=CARTESIAN_POINT('',(4.5963952096795,-1.23456935960355,7.30323111171487));
#3938=CARTESIAN_POINT('',(4.5963952096795,-1.23456935960355,7.30323111171487));
#3939=CARTESIAN_POINT('Origin',(4.58300560234995,-1.11126133386797,7.30323111171487));
#3940=CARTESIAN_POINT('Origin',(0.,0.,10.8017566198263));
#3941=CARTESIAN_POINT('',(4.70116056230231,-0.741687127224166,14.3002311117149));
#3942=CARTESIAN_POINT('',(4.75930776765241,-5.82847102381266E-16,14.3002311117149));
#3943=CARTESIAN_POINT('Origin',(0.,0.,14.3002311117149));
#3944=CARTESIAN_POINT('',(4.75930776765241,-5.82847102381266E-16,14.3002821279377));
#3945=CARTESIAN_POINT('',(4.75930776765241,-5.82847102381266E-16,10.8017566198263));
#3946=CARTESIAN_POINT('Origin',(0.,0.,14.3002821279377));
#3947=CARTESIAN_POINT('',(4.70116056230231,0.741687127224165,14.3002311117149));
#3948=CARTESIAN_POINT('Origin',(0.,0.,14.3002311117149));
#3949=CARTESIAN_POINT('',(4.70116056230231,0.741687127224165,7.30323111171487));
#3950=CARTESIAN_POINT('',(4.70116056230231,0.741687127224165,7.30323111171487));
#3951=CARTESIAN_POINT('Origin',(0.,0.,7.30323111171487));
#3952=CARTESIAN_POINT('Origin',(0.,0.,7.30323111171487));
#3953=CARTESIAN_POINT('Origin',(0.,0.,7.30323111171487));
#3954=CARTESIAN_POINT('Origin',(0.,0.,7.30323111171487));
#3955=CARTESIAN_POINT('Origin',(0.,0.,7.30323111171487));
#3956=CARTESIAN_POINT('Origin',(0.,0.,7.30323111171487));
#3957=CARTESIAN_POINT('Origin',(0.,0.,7.30323111171487));
#3958=CARTESIAN_POINT('Origin',(0.,0.,7.30323111171487));
#3959=CARTESIAN_POINT('Origin',(0.,0.,7.30323111171487));
#3960=CARTESIAN_POINT('Origin',(0.,0.,7.30323111171487));
#3961=CARTESIAN_POINT('Origin',(0.,0.,7.30323111171487));
#3962=CARTESIAN_POINT('Origin',(0.,0.,7.30323111171487));
#3963=CARTESIAN_POINT('Origin',(0.,0.,7.30323111171487));
#3964=CARTESIAN_POINT('Origin',(0.,0.,7.30323111171487));
#3965=CARTESIAN_POINT('',(4.70116056230231,-0.741687127224166,7.30323111171487));
#3966=CARTESIAN_POINT('Origin',(0.,0.,7.30323111171487));
#3967=CARTESIAN_POINT('',(4.70116056230231,-0.741687127224166,7.30323111171487));
#3968=CARTESIAN_POINT('Origin',(4.63877465489478,-0.848888570088464,7.30323111171487));
#3969=CARTESIAN_POINT('',(4.66517787878367,-0.727698551673083,7.30323111171487));
#3970=CARTESIAN_POINT('Origin',(4.63877465489478,-0.848888570088464,7.30323111171487));
#3971=CARTESIAN_POINT('',(4.66517787878367,-0.727698551673083,14.3002311117149));
#3972=CARTESIAN_POINT('',(4.66517787878367,-0.727698551673083,7.30323111171487));
#3973=CARTESIAN_POINT('Origin',(4.63877465489478,-0.848888570088464,14.3002311117149));
#3974=CARTESIAN_POINT('Origin',(5.13999824000407,0.,14.3002311117149));
#3975=CARTESIAN_POINT('',(4.66517787878367,0.727698551673083,14.3002311117149));
#3976=CARTESIAN_POINT('Origin',(4.84271052295884,4.85722573273506E-16,14.3002311117149));
#3977=CARTESIAN_POINT('Origin',(4.63877465489478,0.848888570088464,14.3002311117149));
#3978=CARTESIAN_POINT('Origin',(4.84271052295884,4.85722573273506E-16,7.30323111171487));
#3979=CARTESIAN_POINT('',(4.66517787878367,0.727698551673083,7.30323111171487));
#3980=CARTESIAN_POINT('Origin',(4.84271052295884,4.85722573273506E-16,7.30323111171487));
#3981=CARTESIAN_POINT('',(4.66517787878367,0.727698551673083,7.30323111171487));
#3982=CARTESIAN_POINT('Origin',(4.63877465489478,0.848888570088464,7.30323111171487));
#3983=CARTESIAN_POINT('Origin',(4.63877465489478,0.848888570088464,7.30323111171487));
#3984=CARTESIAN_POINT('Origin',(-4.75930776765241,0.,14.3002821279377));
#3985=CARTESIAN_POINT('',(6.71146155382814,-8.21916990949615E-16,14.3002821279377));
#3986=CARTESIAN_POINT('Origin',(0.,0.,14.3002821279377));
#3987=CARTESIAN_POINT('Origin',(-6.71146155382814,0.,7.30323111171487));
#3988=CARTESIAN_POINT('',(6.71146155382814,-8.21916990949615E-16,7.30323111171487));
#3989=CARTESIAN_POINT('Origin',(0.,0.,7.30323111171487));
#3990=CARTESIAN_POINT('Origin',(0.,0.,7.18611620816211));
#3991=CARTESIAN_POINT('',(6.94701057265674,-8.50763426144689E-16,7.06900130460935));
#3992=CARTESIAN_POINT('Origin',(0.,0.,7.06900130460935));
#3993=CARTESIAN_POINT('',(6.82923606324244,-8.36340208547153E-16,7.18611620816211));
#3994=CARTESIAN_POINT('Origin',(0.,0.,3.65014826262535));
#3995=CARTESIAN_POINT('',(6.94701057265674,-8.50763426144689E-16,0.231295220641352));
#3996=CARTESIAN_POINT('Origin',(0.,0.,0.231295220641352));
#3997=CARTESIAN_POINT('',(6.94701057265674,-8.5076342614469E-16,3.65014826262535));
#3998=CARTESIAN_POINT('',(6.94701057265674,-8.5076342614469E-16,3.65014826262535));
#3999=CARTESIAN_POINT('Origin',(0.,0.,0.115647610320677));
#4000=CARTESIAN_POINT('',(6.71701073999059,-8.22596570256787E-16,5.20417042793042E-16));
#4001=CARTESIAN_POINT('',(6.83201065632366,8.36679998200738E-16,0.115647610320677));
#4002=CARTESIAN_POINT('Origin',(0.,0.,0.));
#4003=CARTESIAN_POINT('Origin',(-4.88235460250674,0.,0.));
#4004=CARTESIAN_POINT('',(4.88235460250674,-5.97915993626222E-16,1.82145964977565E-16));
#4005=CARTESIAN_POINT('Origin',(0.,0.,0.));
#4006=CARTESIAN_POINT('Origin',(0.,0.,0.0596026238408975));
#4007=CARTESIAN_POINT('',(4.72357304027696,-5.78470860431392E-16,0.119205247681795));
#4008=CARTESIAN_POINT('Origin',(0.,0.,0.119205247681795));
#4009=CARTESIAN_POINT('',(4.80296382139185,-5.88193427028807E-16,0.0596026238408975));
#4010=CARTESIAN_POINT('Origin',(0.,0.,0.0596026238408975));
#4011=CARTESIAN_POINT('',(4.56686254190236,-5.59279359408668E-16,2.16840434497101E-16));
#4012=CARTESIAN_POINT('',(4.64521779108966,5.68875109920029E-16,0.0596026238408975));
#4013=CARTESIAN_POINT('Origin',(0.,0.,0.));
#4014=CARTESIAN_POINT('Origin',(-2.72176037385134,0.,0.));
#4015=CARTESIAN_POINT('',(2.72176037385134,-3.33319512988314E-16,-1.38777878078145E-16));
#4016=CARTESIAN_POINT('Origin',(0.,0.,0.));
#4017=CARTESIAN_POINT('Origin',(0.,0.,0.10956776965426));
#4018=CARTESIAN_POINT('',(2.61128051468949,-3.19789632399034E-16,0.10956776965426));
#4019=CARTESIAN_POINT('Origin',(0.,0.,15.3841467814851));
#4020=CARTESIAN_POINT('',(2.7303795503838,-3.34375057683491E-16,15.4998917859252));
#4021=CARTESIAN_POINT('',(2.61559010295572,3.20317404746622E-16,15.3841467814851));
#4022=CARTESIAN_POINT('Origin',(0.,0.,15.4998917859252));
#4023=CARTESIAN_POINT('Origin',(-4.56694754124435,0.,15.4998917859252));
#4024=CARTESIAN_POINT('',(4.56694754124434,-5.59289768825876E-16,15.4998917859252));
#4025=CARTESIAN_POINT('Origin',(0.,0.,15.4998917859252));
#4026=CARTESIAN_POINT('Origin',(0.,0.,15.4392892165051));
#4027=CARTESIAN_POINT('',(4.72346421955602,-5.78457533736633E-16,15.378686647085));
#4028=CARTESIAN_POINT('Origin',(0.,0.,15.378686647085));
#4029=CARTESIAN_POINT('',(4.64520588040018,-5.68873651281254E-16,15.4392892165051));
#4030=CARTESIAN_POINT('Origin',(0.,0.,15.4392892165051));
#4031=CARTESIAN_POINT('',(4.8865982268606,-5.98435687724396E-16,15.4998917859252));
#4032=CARTESIAN_POINT('',(4.80503122320831,5.88446610730515E-16,15.4392892165051));
#4033=CARTESIAN_POINT('Origin',(0.,0.,15.4998917859252));
#4034=CARTESIAN_POINT('Origin',(-6.72522523865914,0.,15.4998917859252));
#4035=CARTESIAN_POINT('',(6.72522523865914,-8.23602556206891E-16,15.4998917859252));
#4036=CARTESIAN_POINT('Origin',(0.,0.,15.4998917859252));
#4037=CARTESIAN_POINT('Origin',(0.,0.,15.3866394833227));
#4038=CARTESIAN_POINT('',(6.94665463816359,-8.50719836740916E-16,15.2733871807203));
#4039=CARTESIAN_POINT('Origin',(0.,0.,15.2733871807203));
#4040=CARTESIAN_POINT('',(6.83593993841137,-8.37161196473904E-16,15.3866394833227));
#4041=CARTESIAN_POINT('Origin',(0.,0.,14.9017962538623));
#4042=CARTESIAN_POINT('',(6.94665463816359,-8.50719836740916E-16,14.5302053270043));
#4043=CARTESIAN_POINT('Origin',(0.,0.,14.5302053270043));
#4044=CARTESIAN_POINT('',(6.94665463816359,-8.50719836740916E-16,14.9017962538623));
#4045=CARTESIAN_POINT('Origin',(0.,0.,14.415243727471));
#4046=CARTESIAN_POINT('',(6.82905809599587,8.36318413845266E-16,14.415243727471));
#4047=CARTESIAN_POINT('',(0.,0.,0.));
#4048=CARTESIAN_POINT('Origin',(1.2059437743963,0.,3.64739446828387));
#4049=CARTESIAN_POINT('',(3.0940562256037,-1.55537930835193,3.64803845831604));
#4050=CARTESIAN_POINT('',(2.95594377439629,-1.55549966270667,3.64841883122548));
#4051=CARTESIAN_POINT('',(1.2059437743963,-1.5555,3.64739446828386));
#4052=CARTESIAN_POINT('',(2.50004392260581,-0.903577229903434,2.38124738377906));
#4053=CARTESIAN_POINT('Ctrl Pts',(2.50004392260581,-0.903577229903434,2.38124738377906));
#4054=CARTESIAN_POINT('Ctrl Pts',(2.50433411497395,-0.855085523975061,2.34664160862681));
#4055=CARTESIAN_POINT('Ctrl Pts',(2.50862430734209,-0.804491254712249,2.31474615079293));
#4056=CARTESIAN_POINT('Ctrl Pts',(2.51291449971023,-0.752136324784237,2.28582508006303));
#4057=CARTESIAN_POINT('Ctrl Pts',(2.51701568125145,-0.702087969422061,2.25817817026229));
#4058=CARTESIAN_POINT('Ctrl Pts',(2.52111686279267,-0.650431357336844,2.2332493669833));
#4059=CARTESIAN_POINT('Ctrl Pts',(2.5252180443339,-0.59749677222433,2.21122670051386));
#4060=CARTESIAN_POINT('Ctrl Pts',(2.52931555826907,-0.544609525470972,2.18922372848223));
#4061=CARTESIAN_POINT('Ctrl Pts',(2.53341307220424,-0.490447057473864,2.17012195018667));
#4062=CARTESIAN_POINT('Ctrl Pts',(2.53751058613941,-0.435362908197946,2.15406282790206));
#4063=CARTESIAN_POINT('Ctrl Pts',(2.5416060839302,-0.380305862575501,2.13801160736216));
#4064=CARTESIAN_POINT('Ctrl Pts',(2.54570158172099,-0.324328543987199,2.12500022449484));
#4065=CARTESIAN_POINT('Ctrl Pts',(2.54979707951179,-0.267800829156953,2.11512067881188));
#4066=CARTESIAN_POINT('Ctrl Pts',(2.55389220938536,-0.211278192468817,2.10524202065351));
#4067=CARTESIAN_POINT('Ctrl Pts',(2.55798733925893,-0.15420578155813,2.09849473034022));
#4068=CARTESIAN_POINT('Ctrl Pts',(2.5620824691325,-0.0969625372344377,2.09491950347025));
#4069=CARTESIAN_POINT('Ctrl Pts',(2.56618153629185,-0.0396642560697558,
2.09134083917818));
#4070=CARTESIAN_POINT('Ctrl Pts',(2.5702806034512,0.0178046547621242,2.09094035559528));
#4071=CARTESIAN_POINT('Ctrl Pts',(2.57437967061055,0.0750629135762425,2.09370665890727));
#4072=CARTESIAN_POINT('Ctrl Pts',(2.578481068547,0.132353730100148,2.09647453517141));
#4073=CARTESIAN_POINT('Ctrl Pts',(2.58258246648346,0.189433127822244,2.10241272382605));
#4074=CARTESIAN_POINT('Ctrl Pts',(2.58668386441992,0.245925895792555,2.11145804258825));
#4075=CARTESIAN_POINT('Ctrl Pts',(2.59079224810531,0.302514885660727,2.12051876788424));
#4076=CARTESIAN_POINT('Ctrl Pts',(2.59490063179069,0.358514735044393,2.13269706306549));
#4077=CARTESIAN_POINT('Ctrl Pts',(2.59900901547608,0.413562868294999,2.14787921195347));
#4078=CARTESIAN_POINT('Ctrl Pts',(2.60034219013111,0.431426043128821,2.15280583460032));
#4079=CARTESIAN_POINT('Ctrl Pts',(2.60167536478614,0.449189147593446,2.15804838267406));
#4080=CARTESIAN_POINT('Ctrl Pts',(2.60300853944117,0.466840256073619,2.16360188665087));
#4081=CARTESIAN_POINT('Ctrl Pts',(2.60716403457439,0.521858625278663,2.18091211578018));
#4082=CARTESIAN_POINT('Ctrl Pts',(2.61131952970761,0.576023644694694,2.20132138484262));
#4083=CARTESIAN_POINT('Ctrl Pts',(2.61547502484083,0.628963033455763,2.22472593607191));
#4084=CARTESIAN_POINT('Ctrl Pts',(2.61962338251369,0.681811493752981,2.24809028774582));
#4085=CARTESIAN_POINT('Ctrl Pts',(2.62377174018654,0.733438031573039,2.27443950101456));
#4086=CARTESIAN_POINT('Ctrl Pts',(2.6279200978594,0.7834870450404,2.30362056607641));
#4087=CARTESIAN_POINT('Ctrl Pts',(2.63206447609135,0.833488047437554,2.33277363829552));
#4088=CARTESIAN_POINT('Ctrl Pts',(2.6362088543233,0.881914078343766,2.36475291915531));
#4089=CARTESIAN_POINT('Ctrl Pts',(2.64035323255525,0.928432591928899,2.39935874273584));
#4090=CARTESIAN_POINT('Ctrl Pts',(2.64449521160968,0.974924175980639,2.4339445330305));
#4091=CARTESIAN_POINT('Ctrl Pts',(2.64863719066411,1.01951001672808,2.47115354250065));
#4092=CARTESIAN_POINT('Ctrl Pts',(2.65277916971854,1.06188696852165,2.5107431074507));
#4093=CARTESIAN_POINT('Ctrl Pts',(2.65692032641849,1.10425550673423,2.55032481223155));
#4094=CARTESIAN_POINT('Ctrl Pts',(2.66106148311844,1.14441564814524,2.59228577999221));
#4095=CARTESIAN_POINT('Ctrl Pts',(2.66520263981839,1.18209939933818,2.63634488488832));
#4096=CARTESIAN_POINT('Ctrl Pts',(2.66934763312091,1.21981806289667,2.68044480863942));
#4097=CARTESIAN_POINT('Ctrl Pts',(2.67349262642342,1.25505541323187,2.72664635923879));
#4098=CARTESIAN_POINT('Ctrl Pts',(2.67763761972594,1.28758315415597,2.77463455219367));
#4099=CARTESIAN_POINT('Ctrl Pts',(2.68178439590806,1.32012488618732,2.82264338623629));
#4100=CARTESIAN_POINT('Ctrl Pts',(2.68593117209018,1.34995441737378,2.87243994937993));
#4101=CARTESIAN_POINT('Ctrl Pts',(2.69007794827229,1.37688806469823,2.92368215852843));
#4102=CARTESIAN_POINT('Ctrl Pts',(2.69423278474608,1.4038740642702,2.97502396966489));
#4103=CARTESIAN_POINT('Ctrl Pts',(2.69838762121987,1.42795271460861,3.02781656903579));
#4104=CARTESIAN_POINT('Ctrl Pts',(2.70254245769365,1.4489877876146,3.08169610224084));
#4105=CARTESIAN_POINT('Ctrl Pts',(2.70637366513319,1.46838439412368,3.1313788442106));
#4106=CARTESIAN_POINT('Ctrl Pts',(2.71020487257272,1.48519355951164,3.1819852701583));
#4107=CARTESIAN_POINT('Ctrl Pts',(2.71403608001225,1.49934664266485,3.23322071835562));
#4108=CARTESIAN_POINT('Ctrl Pts',(2.71817915439409,1.51465181137774,3.28862682105782));
#4109=CARTESIAN_POINT('Ctrl Pts',(2.72232222877592,1.52691450781882,3.34500138694104));
#4110=CARTESIAN_POINT('Ctrl Pts',(2.72646530315776,1.5360179517072,3.40197828700556));
#4111=CARTESIAN_POINT('Ctrl Pts',(2.73060090241158,1.54510497073757,3.45885238668985));
#4112=CARTESIAN_POINT('Ctrl Pts',(2.73473650166541,1.55104396849635,3.51632615235848));
#4113=CARTESIAN_POINT('Ctrl Pts',(2.73887210091923,1.55376848069945,3.57402036941437));
#4114=CARTESIAN_POINT('Ctrl Pts',(2.74300352433428,1.55649024188075,3.63165633088643));
#4115=CARTESIAN_POINT('Ctrl Pts',(2.74713494774932,1.55600392310557,3.68951178383782));
#4116=CARTESIAN_POINT('Ctrl Pts',(2.75126637116436,1.55229470988028,3.74720119990902));
#4117=CARTESIAN_POINT('Ctrl Pts',(2.75539522175441,1.54858780655053,3.80485469016076));
#4118=CARTESIAN_POINT('Ctrl Pts',(2.75952407234446,1.54166202030053,3.86234182841597));
#4119=CARTESIAN_POINT('Ctrl Pts',(2.76365292293451,1.53155460991275,3.91927813247688));
#4120=CARTESIAN_POINT('Ctrl Pts',(2.76778080002723,1.52144958264269,3.97620101213823));
#4121=CARTESIAN_POINT('Ctrl Pts',(2.77190867711994,1.50816451151997,4.032572801459));
#4122=CARTESIAN_POINT('Ctrl Pts',(2.77603655421266,1.49178807918711,4.08801741003251));
#4123=CARTESIAN_POINT('Ctrl Pts',(2.78016813677092,1.47539694624562,4.14351178948868));
#4124=CARTESIAN_POINT('Ctrl Pts',(2.78429971932918,1.45590905346099,4.19807682245723));
#4125=CARTESIAN_POINT('Ctrl Pts',(2.78843130188743,1.4334631269432,4.25135118336718));
#4126=CARTESIAN_POINT('Ctrl Pts',(2.79256457361284,1.41100802357336,4.30464732510794));
#4127=CARTESIAN_POINT('Ctrl Pts',(2.79669784533826,1.38559270429132,4.35665127207839));
#4128=CARTESIAN_POINT('Ctrl Pts',(2.80083111706367,1.35740294273005,4.40702431305553));
#4129=CARTESIAN_POINT('Ctrl Pts',(2.80497246662991,1.32915808863627,4.45749580035655));
#4130=CARTESIAN_POINT('Ctrl Pts',(2.80911381619615,1.29812823699445,4.50632956924818));
#4131=CARTESIAN_POINT('Ctrl Pts',(2.81325516576239,1.26454328228959,4.55321483525311));
#4132=CARTESIAN_POINT('Ctrl Pts',(2.81719131736937,1.23262241414807,4.59777700325587));
#4133=CARTESIAN_POINT('Ctrl Pts',(2.82112746897635,1.19839396464653,4.64057893014162));
#4134=CARTESIAN_POINT('Ctrl Pts',(2.82506362058333,1.16208710892346,4.68138373383449));
#4135=CARTESIAN_POINT('Ctrl Pts',(2.82921315257594,1.12381204372855,4.72440058259503));
#4136=CARTESIAN_POINT('Ctrl Pts',(2.83336268456856,1.08306535950521,4.7653790955833));
#4137=CARTESIAN_POINT('Ctrl Pts',(2.83751221656118,1.04009256905409,4.80402219482273));
#4138=CARTESIAN_POINT('Ctrl Pts',(2.84165438986481,0.997195985606616,4.84259676523792));
#4139=CARTESIAN_POINT('Ctrl Pts',(2.84579656316844,0.952081515568067,4.87884379743944));
#4140=CARTESIAN_POINT('Ctrl Pts',(2.84993873647208,0.905032885213859,4.91250147035187));
#4141=CARTESIAN_POINT('Ctrl Pts',(2.85407680034561,0.858030931578244,4.94612575164981));
#4142=CARTESIAN_POINT('Ctrl Pts',(2.85821486421914,0.809099040695546,4.97716546230242));
#4143=CARTESIAN_POINT('Ctrl Pts',(2.86235292809268,0.758554187283901,5.00539881104352));
#4144=CARTESIAN_POINT('Ctrl Pts',(2.86648847416359,0.708040087859669,5.03361498121957));
#4145=CARTESIAN_POINT('Ctrl Pts',(2.87062402023451,0.65591542477365,5.05902792115145));
#4146=CARTESIAN_POINT('Ctrl Pts',(2.87475956630543,0.602524480517781,5.08146019215317));
#4147=CARTESIAN_POINT('Ctrl Pts',(2.87889418260464,0.549145539849433,5.10388741983281));
#4148=CARTESIAN_POINT('Ctrl Pts',(2.88302879890385,0.494501362733951,5.12333510754781));
#4149=CARTESIAN_POINT('Ctrl Pts',(2.88716341520306,0.438957034282695,5.13967358830591));
#4150=CARTESIAN_POINT('Ctrl Pts',(2.89130175187135,0.383362726489476,5.15602677059231));
#4151=CARTESIAN_POINT('Ctrl Pts',(2.89544008853964,0.326867148839329,5.16926500674999));
#4152=CARTESIAN_POINT('Ctrl Pts',(2.89957842520793,0.269850104507573,5.17930868621425));
#4153=CARTESIAN_POINT('Ctrl Pts',(2.90371847051207,0.212809518986683,5.18935651251146));
#4154=CARTESIAN_POINT('Ctrl Pts',(2.90785851581621,0.155247555237423,5.19620708965532));
#4155=CARTESIAN_POINT('Ctrl Pts',(2.91199856112035,0.097550542943304,5.19983259638156));
#4156=CARTESIAN_POINT('Ctrl Pts',(2.91614662856738,0.0397417314675851,5.20346512823214));
#4157=CARTESIAN_POINT('Ctrl Pts',(2.92029469601441,-0.0182021292545922,
5.20386009675022));
#4158=CARTESIAN_POINT('Ctrl Pts',(2.92444276346143,-0.0758942242730695,
5.2010418918398));
#4159=CARTESIAN_POINT('Ctrl Pts',(2.92832556269243,-0.129896919511898,5.19840391065973));
#4160=CARTESIAN_POINT('Ctrl Pts',(2.93220836192342,-0.183678700365295,5.19295113580139));
#4161=CARTESIAN_POINT('Ctrl Pts',(2.93609116115441,-0.236929761373951,5.18474431076452));
#4162=CARTESIAN_POINT('Ctrl Pts',(2.94024039722414,-0.293834898607237,5.17597433517856));
#4163=CARTESIAN_POINT('Ctrl Pts',(2.94438963329388,-0.350371063130989,5.16402229316462));
#4164=CARTESIAN_POINT('Ctrl Pts',(2.94853886936362,-0.406155507456992,5.14893299718093));
#4165=CARTESIAN_POINT('Ctrl Pts',(2.95268077025794,-0.461841333946435,5.13387037662161));
#4166=CARTESIAN_POINT('Ctrl Pts',(2.95682267115226,-0.516777579703662,5.11568164538635));
#4167=CARTESIAN_POINT('Ctrl Pts',(2.96096457204658,-0.570590348551148,5.09446285095978));
#4168=CARTESIAN_POINT('Ctrl Pts',(2.96510237801041,-0.624349914882801,5.07326503470012));
#4169=CARTESIAN_POINT('Ctrl Pts',(2.96924018397424,-0.676987723304684,5.04904328073132));
#4170=CARTESIAN_POINT('Ctrl Pts',(2.97337798993807,-0.728145436661753,5.02194329356025));
#4171=CARTESIAN_POINT('Ctrl Pts',(2.97751329306004,-0.779272206164113,4.99485969840537));
#4172=CARTESIAN_POINT('Ctrl Pts',(2.98164859618201,-0.828920196343047,4.96490156436302));
#4173=CARTESIAN_POINT('Ctrl Pts',(2.98578389930398,-0.876753485845831,4.93226161124348));
#4174=CARTESIAN_POINT('Ctrl Pts',(2.98991828809341,-0.924576199211488,4.89962887495188));
#4175=CARTESIAN_POINT('Ctrl Pts',(2.99405267688284,-0.970584578814997,4.86431579004715));
#4176=CARTESIAN_POINT('Ctrl Pts',(2.99818706567227,-1.0144715234176,4.82655848493922));
#4177=CARTESIAN_POINT('Ctrl Pts',(3.00232520117966,-1.05839823980069,4.78876696293002));
#4178=CARTESIAN_POINT('Ctrl Pts',(3.00646333668705,-1.1001992831074,4.74852713370931));
#4179=CARTESIAN_POINT('Ctrl Pts',(3.01060147219444,-1.13960159336577,4.70611466663573));
#4180=CARTESIAN_POINT('Ctrl Pts',(3.01474133040711,-1.17902030680078,4.66368454325762));
#4181=CARTESIAN_POINT('Ctrl Pts',(3.01888118861977,-1.21603796238855,4.61908037948236));
#4182=CARTESIAN_POINT('Ctrl Pts',(3.02302104683244,-1.25042144777123,4.57261144443255));
#4183=CARTESIAN_POINT('Ctrl Pts',(3.02716895377351,-1.28487178165969,4.52605216429879));
#4184=CARTESIAN_POINT('Ctrl Pts',(3.03131686071459,-1.31667742338716,4.47762130385618));
#4185=CARTESIAN_POINT('Ctrl Pts',(3.03546476765566,-1.34564884130241,4.42765688946119));
#4186=CARTESIAN_POINT('Ctrl Pts',(3.03934941234561,-1.37278148105623,4.38086365137199));
#4187=CARTESIAN_POINT('Ctrl Pts',(3.04323405703555,-1.39742853975662,4.332725917409));
#4188=CARTESIAN_POINT('Ctrl Pts',(3.04711870172549,-1.41947265623265,4.28353724173008));
#4189=CARTESIAN_POINT('Ctrl Pts',(3.05165528585028,-1.44521632053973,4.2260934899805));
#4190=CARTESIAN_POINT('Ctrl Pts',(3.05619186997507,-1.46750340567384,4.16700868888048));
#4191=CARTESIAN_POINT('Ctrl Pts',(3.06072845409986,-1.48614312745068,4.10669704255393));
#4192=CARTESIAN_POINT('Ctrl Pts',(3.06525141942865,-1.50472689290411,4.04656645139699));
#4193=CARTESIAN_POINT('Ctrl Pts',(3.06977438475743,-1.51968497676747,3.98521668123109));
#4194=CARTESIAN_POINT('Ctrl Pts',(3.07429735008621,-1.53087461175201,3.92308119827488));
#4195=CARTESIAN_POINT('Ctrl Pts',(3.07879909482774,-1.54201174785402,3.86123723898547));
#4196=CARTESIAN_POINT('Ctrl Pts',(3.08330083956928,-1.54941557119281,3.79861525544587));
#4197=CARTESIAN_POINT('Ctrl Pts',(3.08780258431081,-1.55299366908022,3.73566062146132));
#4198=CARTESIAN_POINT('Ctrl Pts',(3.08988713140844,-1.55465051858958,3.70650927968396));
#4199=CARTESIAN_POINT('Ctrl Pts',(3.09197167850607,-1.55548775667919,3.67728683394445));
#4200=CARTESIAN_POINT('Ctrl Pts',(3.0940562256037,-1.55549986667069,3.64803850823206));
#4201=CARTESIAN_POINT('',(2.5,0.903606778650208,2.38126847156104));
#4202=CARTESIAN_POINT('Origin',(2.5,0.,3.64739446828387));
#4203=CARTESIAN_POINT('Ctrl Pts',(2.5,0.903606778650211,2.38126847156104));
#4204=CARTESIAN_POINT('Ctrl Pts',(2.50424458524762,0.951845303079998,2.41569526461296));
#4205=CARTESIAN_POINT('Ctrl Pts',(2.50848917049525,0.998152286150711,2.45290980505556));
#4206=CARTESIAN_POINT('Ctrl Pts',(2.51273375574287,1.0422040353451,2.49266896033386));
#4207=CARTESIAN_POINT('Ctrl Pts',(2.51697626655841,1.08623425537784,2.53240868434561));
#4208=CARTESIAN_POINT('Ctrl Pts',(2.52121877737395,1.12801106716945,2.57469023195135));
#4209=CARTESIAN_POINT('Ctrl Pts',(2.52546128818949,1.16724434287761,2.61923062238177));
#4210=CARTESIAN_POINT('Ctrl Pts',(2.52970274247019,1.20646784811627,2.66375992068391));
#4211=CARTESIAN_POINT('Ctrl Pts',(2.53394419675089,1.24314875403151,2.71054658023801));
#4212=CARTESIAN_POINT('Ctrl Pts',(2.53818565103159,1.27703555050152,2.759272600095));
#4213=CARTESIAN_POINT('Ctrl Pts',(2.54242733583174,1.31092418869024,2.80800126816995));
#4214=CARTESIAN_POINT('Ctrl Pts',(2.5466690206319,1.34201813870961,2.85866910663541));
#4215=CARTESIAN_POINT('Ctrl Pts',(2.55091070543205,1.37010880618714,2.91092850898334));
#4216=CARTESIAN_POINT('Ctrl Pts',(2.55515390773845,1.39820952338907,2.96320660766845));
#4217=CARTESIAN_POINT('Ctrl Pts',(2.55939711004484,1.42330459453235,3.01707697287856));
#4218=CARTESIAN_POINT('Ctrl Pts',(2.56364031235124,1.4452318670257,3.07216833837198));
#4219=CARTESIAN_POINT('Ctrl Pts',(2.56788991506085,1.46719221439397,3.12734280312106));
#4220=CARTESIAN_POINT('Ctrl Pts',(2.57213951777047,1.48597504305494,3.18374149258933));
#4221=CARTESIAN_POINT('Ctrl Pts',(2.57638912048009,1.50146706506278,3.24097485442182));
#4222=CARTESIAN_POINT('Ctrl Pts',(2.58064201363542,1.51697108246427,3.29825253175462));
#4223=CARTESIAN_POINT('Ctrl Pts',(2.58489490679076,1.52917911615244,3.35636569304));
#4224=CARTESIAN_POINT('Ctrl Pts',(2.58914779994609,1.53802901468287,3.41491436162175));
#4225=CARTESIAN_POINT('Ctrl Pts',(2.59340971679372,1.54689769072741,3.47358725744138));
#4226=CARTESIAN_POINT('Ctrl Pts',(2.59767163364135,1.55239394856735,3.5326970219068));
#4227=CARTESIAN_POINT('Ctrl Pts',(2.60193355048897,1.55450758299866,3.59183887090921));
#4228=CARTESIAN_POINT('Ctrl Pts',(2.60496488051634,1.5560109261533,3.63390408925219));
#4229=CARTESIAN_POINT('Ctrl Pts',(2.60799621054371,1.55580413569242,3.67598547779199));
#4230=CARTESIAN_POINT('Ctrl Pts',(2.61102754057108,1.55389953165917,3.71793874877079));
#4231=CARTESIAN_POINT('Ctrl Pts',(2.61513472499091,1.55131896143399,3.77478172507797));
#4232=CARTESIAN_POINT('Ctrl Pts',(2.61924190941074,1.5456085090895,3.83162701942664));
#4233=CARTESIAN_POINT('Ctrl Pts',(2.62334909383056,1.53676371753942,3.88809662127468));
#4234=CARTESIAN_POINT('Ctrl Pts',(2.62746184330188,1.52790694169175,3.94464273691165));
#4235=CARTESIAN_POINT('Ctrl Pts',(2.6315745927732,1.51590728810265,4.00081160376279));
#4236=CARTESIAN_POINT('Ctrl Pts',(2.63568734224451,1.50081279014695,4.05622355106948));
#4237=CARTESIAN_POINT('Ctrl Pts',(2.63978159373098,1.48578618297733,4.1113862710967));
#4238=CARTESIAN_POINT('Ctrl Pts',(2.64387584521744,1.46769260897502,4.16579833998209));
#4239=CARTESIAN_POINT('Ctrl Pts',(2.64797009670391,1.44663091606903,4.21909302755551));
#4240=CARTESIAN_POINT('Ctrl Pts',(2.65206136756637,1.42558455612138,4.27234891648024));
#4241=CARTESIAN_POINT('Ctrl Pts',(2.65615263842883,1.40157455173156,4.32448854122649));
#4242=CARTESIAN_POINT('Ctrl Pts',(2.66024390929129,1.3747491713709,4.37516157788351));
#4243=CARTESIAN_POINT('Ctrl Pts',(2.66433385356855,1.34793248907838,4.42581818392448));
#4244=CARTESIAN_POINT('Ctrl Pts',(2.66842379784581,1.31830248987026,4.47500867441784));
#4245=CARTESIAN_POINT('Ctrl Pts',(2.67251374212306,1.28605401101196,4.52240608578392));
#4246=CARTESIAN_POINT('Ctrl Pts',(2.67664218704132,1.25350196148786,4.57024967210879));
#4247=CARTESIAN_POINT('Ctrl Pts',(2.68077063195958,1.21828215147022,4.61626576508543));
#4248=CARTESIAN_POINT('Ctrl Pts',(2.68489907687784,1.18063904171931,4.66014898106973));
#4249=CARTESIAN_POINT('Ctrl Pts',(2.68899394060087,1.1433021248915,4.70367524646555));
#4250=CARTESIAN_POINT('Ctrl Pts',(2.6930888043239,1.10358160406715,4.74510285780619));
#4251=CARTESIAN_POINT('Ctrl Pts',(2.69718366804694,1.0617538575275,4.78417017000583));
#4252=CARTESIAN_POINT('Ctrl Pts',(2.70132890356281,1.0194115789482,4.82371805755303));
#4253=CARTESIAN_POINT('Ctrl Pts',(2.70547413907868,0.974910298315913,4.86084680903068));
#4254=CARTESIAN_POINT('Ctrl Pts',(2.70961937459455,0.928569653750268,4.89532821978437));
#4255=CARTESIAN_POINT('Ctrl Pts',(2.71376461011042,0.882229009184622,4.92980963053806));
#4256=CARTESIAN_POINT('Ctrl Pts',(2.71790984562629,0.834049506379408,4.96164345442314));
#4257=CARTESIAN_POINT('Ctrl Pts',(2.72205508114216,0.78437668455737,4.99064927163385));
#4258=CARTESIAN_POINT('Ctrl Pts',(2.72620925196883,0.734596789904449,5.01971761267242));
#4259=CARTESIAN_POINT('Ctrl Pts',(2.7303634227955,0.68309621457768,5.04607495812686));
#4260=CARTESIAN_POINT('Ctrl Pts',(2.73451759362218,0.630201320826852,5.06951490805966));
#4261=CARTESIAN_POINT('Ctrl Pts',(2.73866438607905,0.577400375568407,5.09291322546801));
#4262=CARTESIAN_POINT('Ctrl Pts',(2.74281117853593,0.523210498602565,5.11340422484302));
#4263=CARTESIAN_POINT('Ctrl Pts',(2.74695797099281,0.467983399567045,5.13082690278491));
#4264=CARTESIAN_POINT('Ctrl Pts',(2.75110063850411,0.412811236673221,5.14823224983814));
#4265=CARTESIAN_POINT('Ctrl Pts',(2.75524330601541,0.356604388684665,5.16257516809759));
#4266=CARTESIAN_POINT('Ctrl Pts',(2.75938597352671,0.299733729231273,5.17374303318021));
#4267=CARTESIAN_POINT('Ctrl Pts',(2.76352609926199,0.242897963352565,5.184904046105));
#4268=CARTESIAN_POINT('Ctrl Pts',(2.76766622499728,0.185399701714438,5.19289376819827));
#4269=CARTESIAN_POINT('Ctrl Pts',(2.77180635073256,0.127622009920947,5.19765021253504));
#4270=CARTESIAN_POINT('Ctrl Pts',(2.77594551424784,0.0698577464276025,5.20240555141119));
#4271=CARTESIAN_POINT('Ctrl Pts',(2.78008467776312,0.0118146987145777,5.20392906193616));
#4272=CARTESIAN_POINT('Ctrl Pts',(2.78422384127839,-0.0461191024158946,
5.20221062410177));
#4273=CARTESIAN_POINT('Ctrl Pts',(2.78836663579256,-0.104103724821433,5.20049067880196));
#4274=CARTESIAN_POINT('Ctrl Pts',(2.79250943030673,-0.161978389084661,5.19552311584121));
#4275=CARTESIAN_POINT('Ctrl Pts',(2.79665222482089,-0.219356586646865,5.18734996695733));
#4276=CARTESIAN_POINT('Ctrl Pts',(2.80079668623878,-0.276757871024192,5.17917352950768));
#4277=CARTESIAN_POINT('Ctrl Pts',(2.80494114765667,-0.333661780046128,5.16778903477395));
#4278=CARTESIAN_POINT('Ctrl Pts',(2.80908560907455,-0.389691619463311,5.15328978062137));
#4279=CARTESIAN_POINT('Ctrl Pts',(2.81323796249252,-0.445828152477676,5.13876291658096));
#4280=CARTESIAN_POINT('Ctrl Pts',(2.81739031591049,-0.501086793044878,5.1211095972325));
#4281=CARTESIAN_POINT('Ctrl Pts',(2.82154266932845,-0.555106538707374,5.10047291788125));
#4282=CARTESIAN_POINT('Ctrl Pts',(2.82538932012338,-0.605149267896918,5.08135554249413));
#4283=CARTESIAN_POINT('Ctrl Pts',(2.82923597091831,-0.654128713604237,5.05967858632401));
#4284=CARTESIAN_POINT('Ctrl Pts',(2.83308262171324,-0.701776811900782,5.03559098040972));
#4285=CARTESIAN_POINT('Ctrl Pts',(2.83723812440405,-0.753250629317283,5.00956935366784));
#4286=CARTESIAN_POINT('Ctrl Pts',(2.84139362709486,-0.803378780995949,4.98062856210417));
#4287=CARTESIAN_POINT('Ctrl Pts',(2.84554912978567,-0.851810797414874,4.94893148865918));
#4288=CARTESIAN_POINT('Ctrl Pts',(2.84969749536435,-0.900159631423033,4.91728885521438));
#4289=CARTESIAN_POINT('Ctrl Pts',(2.85384586094303,-0.946817682329859,4.88289961882828));
#4290=CARTESIAN_POINT('Ctrl Pts',(2.85799422652171,-0.991458942442055,4.84597254894932));
#4291=CARTESIAN_POINT('Ctrl Pts',(2.86213861286569,-1.03605738133995,4.80908090060571));
#4292=CARTESIAN_POINT('Ctrl Pts',(2.86628299920966,-1.07864246529873,4.76965657176451));
#4293=CARTESIAN_POINT('Ctrl Pts',(2.87042738555364,-1.11891851883289,4.72795062055584));
#4294=CARTESIAN_POINT('Ctrl Pts',(2.87456937291235,-1.15917125850318,4.68626881090982));
#4295=CARTESIAN_POINT('Ctrl Pts',(2.87871136027106,-1.19711725811529,4.64230836973604));
#4296=CARTESIAN_POINT('Ctrl Pts',(2.88285334762977,-1.23249683959237,4.59635800309163));
#4297=CARTESIAN_POINT('Ctrl Pts',(2.88699451281254,-1.26786939829556,4.55041675750012));
#4298=CARTESIAN_POINT('Ctrl Pts',(2.89113567799531,-1.30067623431274,4.50248678159935));
#4299=CARTESIAN_POINT('Ctrl Pts',(2.89527684317808,-1.33069860539263,4.45288901923136));
#4300=CARTESIAN_POINT('Ctrl Pts',(2.89942184517836,-1.36074879240209,4.40324530420159));
#4301=CARTESIAN_POINT('Ctrl Pts',(2.90356684717864,-1.38800908947886,4.35193115929336));
#4302=CARTESIAN_POINT('Ctrl Pts',(2.90771184917892,-1.41230542657339,4.29929448521236));
#4303=CARTESIAN_POINT('Ctrl Pts',(2.91185863419015,-1.43661221496202,4.24663516897921));
#4304=CARTESIAN_POINT('Ctrl Pts',(2.91600541920137,-1.45795230958072,4.19265267234785));
#4305=CARTESIAN_POINT('Ctrl Pts',(2.9201522042126,-1.47620006451291,4.13771438377995));
#4306=CARTESIAN_POINT('Ctrl Pts',(2.92430704962584,-1.49448328890885,4.08266930773916));
#4307=CARTESIAN_POINT('Ctrl Pts',(2.92846189503908,-1.50966202478595,4.02666522918671));
#4308=CARTESIAN_POINT('Ctrl Pts',(2.93261674045232,-1.52166098851936,3.97008330604912));
#4309=CARTESIAN_POINT('Ctrl Pts',(2.93644788106299,-1.53272511068825,3.91790969138922));
#4310=CARTESIAN_POINT('Ctrl Pts',(2.94027902167365,-1.54108617161881,3.86524520012915));
#4311=CARTESIAN_POINT('Ctrl Pts',(2.94411016228431,-1.54672433177784,3.8123917151894));
#4312=CARTESIAN_POINT('Ctrl Pts',(2.94805469965497,-1.55252937411617,3.75797383610294));
#4313=CARTESIAN_POINT('Ctrl Pts',(2.95199923702563,-1.5554635597827,3.7032412811352));
#4314=CARTESIAN_POINT('Ctrl Pts',(2.95594377439629,-1.55549966270667,3.64841883122548));
#4315=CARTESIAN_POINT('Origin',(1.2059437743963,0.,3.64739446828387));
#4316=CARTESIAN_POINT('',(3.7940562256037,-1.55549937976475,3.64600538531537));
#4317=CARTESIAN_POINT('',(3.65594309057409,-1.55328922867419,3.64812360962188));
#4318=CARTESIAN_POINT('',(1.2059437743963,-1.5555,3.64739446828386));
#4319=CARTESIAN_POINT('Ctrl Pts',(3.0940562256037,-1.55320831614475,3.64803755943733));
#4320=CARTESIAN_POINT('Ctrl Pts',(3.11541956450132,-1.55211225787393,3.34872916974666));
#4321=CARTESIAN_POINT('Ctrl Pts',(3.1737920835893,-1.32451511527677,2.5293530162389));
#4322=CARTESIAN_POINT('Ctrl Pts',(3.26917378286765,0.00194386449727044,
1.80949553386703));
#4323=CARTESIAN_POINT('Ctrl Pts',(3.38020132343871,1.54419526187211,2.6507072563878));
#4324=CARTESIAN_POINT('Ctrl Pts',(3.4912288640098,1.67560476579265,4.40256135417452));
#4325=CARTESIAN_POINT('Ctrl Pts',(3.60225640458087,0.276097817182276,5.46444788548381));
#4326=CARTESIAN_POINT('Ctrl Pts',(3.70319885844552,-1.22562677556159,4.92053574953289));
#4327=CARTESIAN_POINT('Ctrl Pts',(3.76713213211979,-1.55162911722742,4.02218696309102));
#4328=CARTESIAN_POINT('Ctrl Pts',(3.7940562256037,-1.5548981372976,3.64600592223341));
#4329=CARTESIAN_POINT('Ctrl Pts',(2.95594474730389,-1.55731930826876,3.64840649193144));
#4330=CARTESIAN_POINT('Ctrl Pts',(2.98900906582105,-1.55406984475527,3.18832795677562));
#4331=CARTESIAN_POINT('Ctrl Pts',(3.05908256452858,-1.09493216072152,2.20731900520876));
#4332=CARTESIAN_POINT('Ctrl Pts',(3.16616524342647,0.571437519320519,1.90065774706199));
#4333=CARTESIAN_POINT('Ctrl Pts',(3.27719278399755,1.77703909951801,3.17828914298809));
#4334=CARTESIAN_POINT('Ctrl Pts',(3.38822032456863,1.35908642417454,4.88467959896744));
#4335=CARTESIAN_POINT('Ctrl Pts',(3.4992478651397,-0.300609421841399,5.4605432395681));
#4336=CARTESIAN_POINT('Ctrl Pts',(3.58848878714152,-1.41386361340158,4.59192891748905));
#4337=CARTESIAN_POINT('Ctrl Pts',(3.64072052895299,-1.55417851871196,3.86136782353057));
#4338=CARTESIAN_POINT('Ctrl Pts',(3.65594309057409,-1.55328922867419,3.64812360962188));
#4339=CARTESIAN_POINT('Origin',(1.2059437743963,0.,3.64739446828387));
#4340=CARTESIAN_POINT('',(4.49405622566528,-1.55549997006787,3.64769962209175));
#4341=CARTESIAN_POINT('',(4.35539415465377,-1.5555,3.64739446822634));
#4342=CARTESIAN_POINT('',(1.2059437743963,-1.5555,3.64739446828386));
#4343=CARTESIAN_POINT('Ctrl Pts',(3.7940562256037,-1.55549937976475,3.64600538531537));
#4344=CARTESIAN_POINT('Ctrl Pts',(3.79924672256038,-1.55543459285259,3.57345680185877));
#4345=CARTESIAN_POINT('Ctrl Pts',(3.80443721951705,-1.55029041969612,3.5011332527424));
#4346=CARTESIAN_POINT('Ctrl Pts',(3.80962771647373,-1.54018379952585,3.42964664699029));
#4347=CARTESIAN_POINT('Ctrl Pts',(3.8145223062235,-1.5306533518822,3.36223545097562));
#4348=CARTESIAN_POINT('Ctrl Pts',(3.81941689597326,-1.51671067473822,3.29556811307793));
#4349=CARTESIAN_POINT('Ctrl Pts',(3.82431148572303,-1.49849211920356,3.23013960769526));
#4350=CARTESIAN_POINT('Ctrl Pts',(3.82845990987145,-1.48305092809396,3.17468548271223));
#4351=CARTESIAN_POINT('Ctrl Pts',(3.83260833401987,-1.46449498927746,3.11997351657148));
#4352=CARTESIAN_POINT('Ctrl Pts',(3.83675675816829,-1.44291390367817,3.06637836130212));
#4353=CARTESIAN_POINT('Ctrl Pts',(3.84089781910633,-1.42137112324431,3.0128783343005));
#4354=CARTESIAN_POINT('Ctrl Pts',(3.84503888004438,-1.39681404658781,2.96049166264528));
#4355=CARTESIAN_POINT('Ctrl Pts',(3.84917994098242,-1.36938210802426,2.90957816850252));
#4356=CARTESIAN_POINT('Ctrl Pts',(3.85331689052468,-1.34197740488623,2.85871522312702));
#4357=CARTESIAN_POINT('Ctrl Pts',(3.85745384006693,-1.3117037407644,2.8093230134315));
#4358=CARTESIAN_POINT('Ctrl Pts',(3.86159078960919,-1.27874802547169,2.7617400563645));
#4359=CARTESIAN_POINT('Ctrl Pts',(3.86572522133919,-1.24581236754324,2.71418605903009));
#4360=CARTESIAN_POINT('Ctrl Pts',(3.86985965306919,-1.21019819009308,2.66843955871357));
#4361=CARTESIAN_POINT('Ctrl Pts',(3.87399408479919,-1.1721364451885,2.62481126684701));
#4362=CARTESIAN_POINT('Ctrl Pts',(3.87812758870062,-1.13408324191102,2.58119276582428));
#4363=CARTESIAN_POINT('Ctrl Pts',(3.88226109260206,-1.09358390378638,2.5396919216926));
#4364=CARTESIAN_POINT('Ctrl Pts',(3.88639459650349,-1.05090908617977,2.50058570367453));
#4365=CARTESIAN_POINT('Ctrl Pts',(3.89053183292945,-1.0081957335174,2.46144417302066));
#4366=CARTESIAN_POINT('Ctrl Pts',(3.89466906935541,-0.96330335971897,2.42470194310739));
#4367=CARTESIAN_POINT('Ctrl Pts',(3.89880630578137,-0.91653786376006,2.39059751002285));
#4368=CARTESIAN_POINT('Ctrl Pts',(3.90294525567577,-0.86975299950965,2.35647895232384));
#4369=CARTESIAN_POINT('Ctrl Pts',(3.90708420557016,-0.82109390399685,2.32500065384954));
#4370=CARTESIAN_POINT('Ctrl Pts',(3.91122315546455,-0.770895120881121,2.29635747300888));
#4371=CARTESIAN_POINT('Ctrl Pts',(3.91537015021836,-0.720598766602835,2.26765861853869));
#4372=CARTESIAN_POINT('Ctrl Pts',(3.91951714497217,-0.668757211424592,2.2418061280752));
#4373=CARTESIAN_POINT('Ctrl Pts',(3.92366413972598,-0.61572840390472,2.21894818556094));
#4374=CARTESIAN_POINT('Ctrl Pts',(3.92755576858202,-0.565965033127231,2.1974978018592));
#4375=CARTESIAN_POINT('Ctrl Pts',(3.93144739743807,-0.515156658330791,2.17868417709864));
#4376=CARTESIAN_POINT('Ctrl Pts',(3.93533902629412,-0.463610415301871,2.16258955422155));
#4377=CARTESIAN_POINT('Ctrl Pts',(3.93948744510044,-0.40866288256262,2.14543292426175));
#4378=CARTESIAN_POINT('Ctrl Pts',(3.94363586390677,-0.352646623653681,2.13129460873933));
#4379=CARTESIAN_POINT('Ctrl Pts',(3.9477842827131,-0.295924871440223,2.12030287952336));
#4380=CARTESIAN_POINT('Ctrl Pts',(3.95192533826022,-0.239303797818583,2.10933066013874));
#4381=CARTESIAN_POINT('Ctrl Pts',(3.95606639380735,-0.181980223358909,2.10149403971228));
#4382=CARTESIAN_POINT('Ctrl Pts',(3.96020744935448,-0.124331997913654,2.0968713938684));
#4383=CARTESIAN_POINT('Ctrl Pts',(3.96434439347988,-0.0667410081572655,
2.09225333759024));
#4384=CARTESIAN_POINT('Ctrl Pts',(3.96848133760527,-0.00882652245795808,
2.09084297499291));
#4385=CARTESIAN_POINT('Ctrl Pts',(3.97261828173067,0.0490257099392183,2.09266724791209));
#4386=CARTESIAN_POINT('Ctrl Pts',(3.97675270802733,0.10684273228551,2.0944904105415));
#4387=CARTESIAN_POINT('Ctrl Pts',(3.98088713432399,0.164597057061208,2.09954428982219));
#4388=CARTESIAN_POINT('Ctrl Pts',(3.98502156062065,0.221902358276826,2.1078037455945));
#4389=CARTESIAN_POINT('Ctrl Pts',(3.98915505908169,0.279194799207568,2.11606134780436));
#4390=CARTESIAN_POINT('Ctrl Pts',(3.99328855754272,0.336037901517856,2.12752302405912));
#4391=CARTESIAN_POINT('Ctrl Pts',(3.99742205600376,0.392052103871693,2.14211197059456));
#4392=CARTESIAN_POINT('Ctrl Pts',(4.00155928702243,0.448116887165724,2.15671409097879));
#4393=CARTESIAN_POINT('Ctrl Pts',(4.00569651804109,0.503350769332033,2.17444899447389));
#4394=CARTESIAN_POINT('Ctrl Pts',(4.00983374905976,0.557387348271569,2.1951893884185));
#4395=CARTESIAN_POINT('Ctrl Pts',(4.01397269355601,0.611446307026598,2.21593837221463));
#4396=CARTESIAN_POINT('Ctrl Pts',(4.01811163805227,0.664306497514946,2.23969511520849));
#4397=CARTESIAN_POINT('Ctrl Pts',(4.02225058254852,0.715622597532277,2.26628457117171));
#4398=CARTESIAN_POINT('Ctrl Pts',(4.026397571991,0.76703844164267,2.29292570957317));
#4399=CARTESIAN_POINT('Ctrl Pts',(4.03054456143347,0.816903747256577,2.32241029888278));
#4400=CARTESIAN_POINT('Ctrl Pts',(4.03469155087595,0.864899667938198,2.35451828921629));
#4401=CARTESIAN_POINT('Ctrl Pts',(4.03858322287236,0.909940626698687,2.38464948886733));
#4402=CARTESIAN_POINT('Ctrl Pts',(4.04247489486878,0.953335299435898,2.41709037054296));
#4403=CARTESIAN_POINT('Ctrl Pts',(4.04636656686519,0.994847796632108,2.4516277219925));
#4404=CARTESIAN_POINT('Ctrl Pts',(4.0505149831588,1.03909898735835,2.48844359743718));
#4405=CARTESIAN_POINT('Ctrl Pts',(4.05466339945241,1.08139645579429,2.5277962696892));
#4406=CARTESIAN_POINT('Ctrl Pts',(4.05881181574603,1.12143520301905,2.56945043660615));
#4407=CARTESIAN_POINT('Ctrl Pts',(4.06295286868638,1.16140288229428,2.61103066823696));
#4408=CARTESIAN_POINT('Ctrl Pts',(4.06709392162673,1.19911944019534,2.65490391383242));
#4409=CARTESIAN_POINT('Ctrl Pts',(4.07123497456709,1.23431383195747,2.70079549604776));
#4410=CARTESIAN_POINT('Ctrl Pts',(4.0753719160303,1.26947328068963,2.74664151444305));
#4411=CARTESIAN_POINT('Ctrl Pts',(4.07950885749352,1.30211520951442,2.79450148797202));
#4412=CARTESIAN_POINT('Ctrl Pts',(4.08364579895674,1.33200746762012,2.84406616914072));
#4413=CARTESIAN_POINT('Ctrl Pts',(4.08778022254044,1.36188153230803,2.89360068360374));
#4414=CARTESIAN_POINT('Ctrl Pts',(4.09191464612414,1.38900897537653,2.94483740401325));
#4415=CARTESIAN_POINT('Ctrl Pts',(4.09604906970783,1.41320106171707,2.99743830886868));
#4416=CARTESIAN_POINT('Ctrl Pts',(4.10018256540968,1.43738771866765,3.05002740858995));
#4417=CARTESIAN_POINT('Ctrl Pts',(4.10431606111153,1.45864010930287,3.10397961210197));
#4418=CARTESIAN_POINT('Ctrl Pts',(4.10844955681337,1.4768165506152,3.15893451513619));
#4419=CARTESIAN_POINT('Ctrl Pts',(4.11258678502196,1.49500940507867,3.21393904191767));
#4420=CARTESIAN_POINT('Ctrl Pts',(4.11672401323054,1.51012059463378,3.26994758241584));
#4421=CARTESIAN_POINT('Ctrl Pts',(4.12086124143913,1.52205797546509,3.3265833566884));
#4422=CARTESIAN_POINT('Ctrl Pts',(4.12500018309285,1.53400030019751,3.38324258683218));
#4423=CARTESIAN_POINT('Ctrl Pts',(4.12913912474658,1.5427661155984,3.44052905299624));
#4424=CARTESIAN_POINT('Ctrl Pts',(4.1332780664003,1.5483148227319,3.49805773566702));
#4425=CARTESIAN_POINT('Ctrl Pts',(4.13742505298203,1.55387431497743,3.55569823777109));
#4426=CARTESIAN_POINT('Ctrl Pts',(4.14157203956375,1.55620418080109,3.6135813750954));
#4427=CARTESIAN_POINT('Ctrl Pts',(4.14571902614548,1.55531598818641,3.67131991272536));
#4428=CARTESIAN_POINT('Ctrl Pts',(4.14961071990908,1.55448247363523,3.72550400577357));
#4429=CARTESIAN_POINT('Ctrl Pts',(4.15350241367268,1.55081545093387,3.77956041061298));
#4430=CARTESIAN_POINT('Ctrl Pts',(4.15739410743628,1.5443658084111,3.83317525257204));
#4431=CARTESIAN_POINT('Ctrl Pts',(4.16154252658954,1.53749069896047,3.89032693273814));
#4432=CARTESIAN_POINT('Ctrl Pts',(4.16569094574279,1.52742442723014,3.94721615662609));
#4433=CARTESIAN_POINT('Ctrl Pts',(4.16983936489605,1.51419888969869,4.00345903045659));
#4434=CARTESIAN_POINT('Ctrl Pts',(4.17398042076164,1.50099682699795,4.05960207530557));
#4435=CARTESIAN_POINT('Ctrl Pts',(4.17812147662723,1.48464674700967,4.115100544536));
#4436=CARTESIAN_POINT('Ctrl Pts',(4.18226253249283,1.46523204945129,4.16957766531415));
#4437=CARTESIAN_POINT('Ctrl Pts',(4.18639947691915,1.44583662773766,4.22400069858879));
#4438=CARTESIAN_POINT('Ctrl Pts',(4.19053642134547,1.42338279090196,4.27740390454189));
#4439=CARTESIAN_POINT('Ctrl Pts',(4.1946733657718,1.39800409065943,4.32942438881485));
#4440=CARTESIAN_POINT('Ctrl Pts',(4.19880779235131,1.37264083652224,4.38141321213309));
#4441=CARTESIAN_POINT('Ctrl Pts',(4.20294221893083,1.34435647560062,4.43202051497412));
#4442=CARTESIAN_POINT('Ctrl Pts',(4.20707664551035,1.31333230115958,4.48090422631366));
#4443=CARTESIAN_POINT('Ctrl Pts',(4.21121014423562,1.28231508921055,4.529776967097));
#4444=CARTESIAN_POINT('Ctrl Pts',(4.21534364296089,1.24855956333046,4.57692644490256));
#4445=CARTESIAN_POINT('Ctrl Pts',(4.21947714168616,1.21229136733348,4.62203793678336));
#4446=CARTESIAN_POINT('Ctrl Pts',(4.22361437293737,1.17599042136089,4.66719016408588));
#4447=CARTESIAN_POINT('Ctrl Pts',(4.22775160418858,1.13717259725465,4.71030032036805));
#4448=CARTESIAN_POINT('Ctrl Pts',(4.23188883543979,1.09610419663964,4.75108638186709));
#4449=CARTESIAN_POINT('Ctrl Pts',(4.23602778015166,1.0550187872851,4.79188933517311));
#4450=CARTESIAN_POINT('Ctrl Pts',(4.24016672486353,1.01168133261274,4.83036592741653));
#4451=CARTESIAN_POINT('Ctrl Pts',(4.2443056695754,0.966393050279938,4.86627293735724));
#4452=CARTESIAN_POINT('Ctrl Pts',(4.24845265920163,0.92101674059282,4.90224974016541));
#4453=CARTESIAN_POINT('Ctrl Pts',(4.25259964882785,0.873682452134044,4.93564667763785));
#4454=CARTESIAN_POINT('Ctrl Pts',(4.25674663845407,0.824721598466709,4.96626312551344));
#4455=CARTESIAN_POINT('Ctrl Pts',(4.26063830830516,0.778775142055065,4.99499459529853));
#4456=CARTESIAN_POINT('Ctrl Pts',(4.26452997815626,0.731396819639839,5.02127767127384));
#4457=CARTESIAN_POINT('Ctrl Pts',(4.26842164800735,0.682877801894672,5.04498459334898));
#4458=CARTESIAN_POINT('Ctrl Pts',(4.27257006638072,0.631157796762306,5.07025555282798));
#4459=CARTESIAN_POINT('Ctrl Pts',(4.27671848475409,0.577924791530181,5.09270459408807));
#4460=CARTESIAN_POINT('Ctrl Pts',(4.28086690312746,0.523518435833337,5.11214997598562));
#4461=CARTESIAN_POINT('Ctrl Pts',(4.2850079582022,0.469208649529545,5.13156084300521));
#4462=CARTESIAN_POINT('Ctrl Pts',(4.28914901327693,0.413730132841133,5.1479784589707));
#4463=CARTESIAN_POINT('Ctrl Pts',(4.29329006835167,0.357444531875432,5.16126819374196));
#4464=CARTESIAN_POINT('Ctrl Pts',(4.29742701198102,0.30121481405313,5.17454473380371));
#4465=CARTESIAN_POINT('Ctrl Pts',(4.30156395561037,0.244180103809134,5.18469942661238));
#4466=CARTESIAN_POINT('Ctrl Pts',(4.30570089923972,0.186717636011615,5.19164728903643));
#4467=CARTESIAN_POINT('Ctrl Pts',(4.30983532501754,0.129290141367093,5.19859092281064));
#4468=CARTESIAN_POINT('Ctrl Pts',(4.31396975079536,0.0714359211261826,5.20233153280199));
#4469=CARTESIAN_POINT('Ctrl Pts',(4.31810417657318,0.0135406585836287,5.20283553131555));
#4470=CARTESIAN_POINT('Ctrl Pts',(4.32223767449341,-0.0443416109675579,
5.20333941672058));
#4471=CARTESIAN_POINT('Ctrl Pts',(4.32637117241365,-0.102264384113827,5.20060812818138));
#4472=CARTESIAN_POINT('Ctrl Pts',(4.33050467033388,-0.159840849343945,5.19466017037935));
#4473=CARTESIAN_POINT('Ctrl Pts',(4.33464190078134,-0.217469305824048,5.18870684160221));
#4474=CARTESIAN_POINT('Ctrl Pts',(4.33877913122879,-0.27475031016035,5.17953109150458));
#4475=CARTESIAN_POINT('Ctrl Pts',(4.34291636167625,-0.331302421324728,5.16720332324701));
#4476=CARTESIAN_POINT('Ctrl Pts',(4.34705530558373,-0.387877953901842,5.15487044936664));
#4477=CARTESIAN_POINT('Ctrl Pts',(4.35119424949121,-0.443723488318946,5.13938309309897));
#4478=CARTESIAN_POINT('Ctrl Pts',(4.35533319339869,-0.498471197309644,5.12086205036795));
#4479=CARTESIAN_POINT('Ctrl Pts',(4.35948018223006,-0.553325320197597,5.10230500802389));
#4480=CARTESIAN_POINT('Ctrl Pts',(4.36362717106142,-0.607076868142607,5.08070268949815));
#4481=CARTESIAN_POINT('Ctrl Pts',(4.36777415989279,-0.659377377398221,5.05622438143004));
#4482=CARTESIAN_POINT('Ctrl Pts',(4.37166583612134,-0.708457964997463,5.03325309949574));
#4483=CARTESIAN_POINT('Ctrl Pts',(4.37555751234988,-0.75626058697706,5.00774967826569));
#4484=CARTESIAN_POINT('Ctrl Pts',(4.37944918857843,-0.80251981524134,4.97988919478188));
#4485=CARTESIAN_POINT('Ctrl Pts',(4.38359760630016,-0.851830855280502,4.95019070070559));
#4486=CARTESIAN_POINT('Ctrl Pts',(4.3877460240219,-0.899594386513456,4.91768906526787));
#4487=CARTESIAN_POINT('Ctrl Pts',(4.39189444174363,-0.945473326109707,4.88257074704535));
#4488=CARTESIAN_POINT('Ctrl Pts',(4.3960354961564,-0.991270832053471,4.84751476271605));
#4489=CARTESIAN_POINT('Ctrl Pts',(4.40017655056918,-1.0351899758604,4.80985162826571));
#4490=CARTESIAN_POINT('Ctrl Pts',(4.40431760498195,-1.07692128200617,4.76981186050577));
#4491=CARTESIAN_POINT('Ctrl Pts',(4.40845454794349,-1.11861115517064,4.72981184628104));
#4492=CARTESIAN_POINT('Ctrl Pts',(4.41259149090503,-1.15811712064239,4.68744023260772));
#4493=CARTESIAN_POINT('Ctrl Pts',(4.41672843386657,-1.1951629199996,4.64296759199605));
#4494=CARTESIAN_POINT('Ctrl Pts',(4.42086285897187,-1.2321861722736,4.59852201864561));
#4495=CARTESIAN_POINT('Ctrl Pts',(4.42499728407717,-1.26675189399725,4.55197835246775));
#4496=CARTESIAN_POINT('Ctrl Pts',(4.42913170918247,-1.298622390327,4.50364217621738));
#4497=CARTESIAN_POINT('Ctrl Pts',(4.43326520642658,-1.33048573417588,4.45531684772954));
#4498=CARTESIAN_POINT('Ctrl Pts',(4.43739870367069,-1.35965476700263,4.40520024231461));
#4499=CARTESIAN_POINT('Ctrl Pts',(4.44153220091481,-1.38593491887239,4.35362718534686));
#4500=CARTESIAN_POINT('Ctrl Pts',(4.44566943068581,-1.41223880158502,4.30200755817217));
#4501=CARTESIAN_POINT('Ctrl Pts',(4.44980666045682,-1.43564835228939,4.24892931577879));
#4502=CARTESIAN_POINT('Ctrl Pts',(4.45394389022782,-1.45601549310078,4.1947509644091));
#4503=CARTESIAN_POINT('Ctrl Pts',(4.45808283345756,-1.47639106908672,4.14055017474754));
#4504=CARTESIAN_POINT('Ctrl Pts',(4.46222177668729,-1.49372156596722,4.08524886536933));
#4505=CARTESIAN_POINT('Ctrl Pts',(4.46636071991703,-1.50790861123553,4.02922148430256));
#4506=CARTESIAN_POINT('Ctrl Pts',(4.47050770807723,-1.52212323209172,3.97308520191481));
#4507=CARTESIAN_POINT('Ctrl Pts',(4.47465469623744,-1.53318209055859,3.91622054035901));
#4508=CARTESIAN_POINT('Ctrl Pts',(4.47880168439765,-1.54103804564489,3.85901202869643));
#4509=CARTESIAN_POINT('Ctrl Pts',(4.4826933659816,-1.54841035406552,3.80532552111992));
#4510=CARTESIAN_POINT('Ctrl Pts',(4.48658504756556,-1.55296246258241,3.7513366184223));
#4511=CARTESIAN_POINT('Ctrl Pts',(4.49047672914951,-1.55469719497037,3.69736327806831));
#4512=CARTESIAN_POINT('Ctrl Pts',(4.49166989463424,-1.55522905318279,3.68081538600245));
#4513=CARTESIAN_POINT('Ctrl Pts',(4.49286306011897,-1.55549672149286,3.66425895728589));
#4514=CARTESIAN_POINT('Ctrl Pts',(4.4940562256037,-1.55549997006771,3.64769962294641));
#4515=CARTESIAN_POINT('Ctrl Pts',(3.6546715967529,-1.55549987088463,3.64802824892936));
#4516=CARTESIAN_POINT('Ctrl Pts',(3.65583554611893,-1.55550678373996,3.63106189683294));
#4517=CARTESIAN_POINT('Ctrl Pts',(3.65700687296806,-1.55523611007452,3.61409701908527));
#4518=CARTESIAN_POINT('Ctrl Pts',(3.65935708872429,-1.55414398231178,3.58031035979871));
#4519=CARTESIAN_POINT('Ctrl Pts',(3.66053568689316,-1.553326734999,3.56349088548048));
#4520=CARTESIAN_POINT('Ctrl Pts',(3.66337304825961,-1.55072111876458,3.52332906623534));
#4521=CARTESIAN_POINT('Ctrl Pts',(3.66503936028455,-1.54867857683863,3.50000800802103));
#4522=CARTESIAN_POINT('Ctrl Pts',(3.66896318495946,-1.54269205754422,3.44576983796235));
#4523=CARTESIAN_POINT('Ctrl Pts',(3.67123284707807,-1.53834370033202,3.41490860768942));
#4524=CARTESIAN_POINT('Ctrl Pts',(3.68315082552336,-1.51100262491104,3.25565012963292));
#4525=CARTESIAN_POINT('Ctrl Pts',(3.69328367884008,-1.4728553502184,3.13040637075574));
#4526=CARTESIAN_POINT('Ctrl Pts',(3.70803836616504,-1.39487416093124,2.9563457391689));
#4527=CARTESIAN_POINT('Ctrl Pts',(3.71267374577518,-1.36701325213118,2.9027478965415));
#4528=CARTESIAN_POINT('Ctrl Pts',(3.7186219360081,-1.32611964739185,2.83414959584725));
#4529=CARTESIAN_POINT('Ctrl Pts',(3.72005913626803,-1.31581933905118,2.8175871968984));
#4530=CARTESIAN_POINT('Ctrl Pts',(3.72256246548942,-1.29708770617275,2.78869391088441));
#4531=CARTESIAN_POINT('Ctrl Pts',(3.72363581372294,-1.28878631801524,2.77628424176131));
#4532=CARTESIAN_POINT('Ctrl Pts',(3.72625693457796,-1.26785639942322,2.74595063821165));
#4533=CARTESIAN_POINT('Ctrl Pts',(3.72779180579342,-1.25502548111744,2.72817088166312));
#4534=CARTESIAN_POINT('Ctrl Pts',(3.73483261797166,-1.19371101295616,2.646886116256));
#4535=CARTESIAN_POINT('Ctrl Pts',(3.74009812593129,-1.14076045336598,2.58689086018623));
#4536=CARTESIAN_POINT('Ctrl Pts',(3.75216359587134,-1.00929016446441,2.45929557370979));
#4537=CARTESIAN_POINT('Ctrl Pts',(3.75893462135127,-0.928279295445408,2.39499531484981));
#4538=CARTESIAN_POINT('Ctrl Pts',(3.76820638574018,-0.814750259645629,2.32195845638415));
#4539=CARTESIAN_POINT('Ctrl Pts',(3.77042440273262,-0.787389467575519,2.30552406392182));
#4540=CARTESIAN_POINT('Ctrl Pts',(3.77449557003691,-0.736979070458635,2.27731757093337));
#4541=CARTESIAN_POINT('Ctrl Pts',(3.77633744759334,-0.714103896334543,2.26525687274259));
#4542=CARTESIAN_POINT('Ctrl Pts',(3.78052407799056,-0.66203132754091,2.23943995787143));
#4543=CARTESIAN_POINT('Ctrl Pts',(3.78287931487905,-0.632685878936419,2.22601145424461));
#4544=CARTESIAN_POINT('Ctrl Pts',(3.79467579654245,-0.48560822553442,2.16416571683606));
#4545=CARTESIAN_POINT('Ctrl Pts',(3.80456766130157,-0.362675252472706,2.12942285856925));
#4546=CARTESIAN_POINT('Ctrl Pts',(3.81907447215377,-0.177330195496224,2.1008599285124));
#4547=CARTESIAN_POINT('Ctrl Pts',(3.82370504365851,-0.117254235714453,2.09514835401263));
#4548=CARTESIAN_POINT('Ctrl Pts',(3.82964856040533,-0.0375065884422887,
2.09222446656055));
#4549=CARTESIAN_POINT('Ctrl Pts',(3.83108561643035,-0.0180072309045984,
2.09187644622304));
#4550=CARTESIAN_POINT('Ctrl Pts',(3.8335889385491,0.0164270910425676,2.09190953556467));
#4551=CARTESIAN_POINT('Ctrl Pts',(3.83466241648109,0.0313576239195768,2.09213887509024));
#4552=CARTESIAN_POINT('Ctrl Pts',(3.83728434998413,0.0682069141321993,2.0932358269107));
#4553=CARTESIAN_POINT('Ctrl Pts',(3.838819886545,0.0901145359934732,2.09435204504922));
#4554=CARTESIAN_POINT('Ctrl Pts',(3.84753727450119,0.2158521755376,2.10342844313732));
#4555=CARTESIAN_POINT('Ctrl Pts',(3.85430539505902,0.31870990806458,2.12133652219784));
#4556=CARTESIAN_POINT('Ctrl Pts',(3.86606195438739,0.490423267156688,2.16936768880612));
#4557=CARTESIAN_POINT('Ctrl Pts',(3.8709835101432,0.560303712190277,2.1944195002446));
#4558=CARTESIAN_POINT('Ctrl Pts',(3.87836259443023,0.658944774022286,2.23795954717948));
#4559=CARTESIAN_POINT('Ctrl Pts',(3.88069634274767,0.689310208044315,2.25255893699471));
#4560=CARTESIAN_POINT('Ctrl Pts',(3.88488549146297,0.742147378174409,2.28010932246872));
#4561=CARTESIAN_POINT('Ctrl Pts',(3.88672620365827,0.764814597393887,2.29265837394579));
#4562=CARTESIAN_POINT('Ctrl Pts',(3.89079627301214,0.813669412320937,2.32132236129602));
#4563=CARTESIAN_POINT('Ctrl Pts',(3.89303318337718,0.839713288787557,2.33765919423335));
#4564=CARTESIAN_POINT('Ctrl Pts',(3.90507091660595,0.975481178202121,2.42853824264551));
#4565=CARTESIAN_POINT('Ctrl Pts',(3.91537836815592,1.07579959823276,2.51610516441578));
#4566=CARTESIAN_POINT('Ctrl Pts',(3.9302395803928,1.20329253551957,2.65986489289857));
#4567=CARTESIAN_POINT('Ctrl Pts',(3.93481226237696,1.24022315403313,2.70666307428741));
#4568=CARTESIAN_POINT('Ctrl Pts',(3.94069738495624,1.28553665769888,2.77140690163977));
#4569=CARTESIAN_POINT('Ctrl Pts',(3.94213095783939,1.29639246572689,2.78755414106253));
#4570=CARTESIAN_POINT('Ctrl Pts',(3.94463099181762,1.31504202698692,2.81645055925576));
#4571=CARTESIAN_POINT('Ctrl Pts',(3.94570457421527,1.32295931239138,2.82911456180249));
#4572=CARTESIAN_POINT('Ctrl Pts',(3.94833055590118,1.34208104326945,2.86070376855959));
#4573=CARTESIAN_POINT('Ctrl Pts',(3.94986991580466,1.35306867879814,2.87975583757066));
#4574=CARTESIAN_POINT('Ctrl Pts',(3.95716047724157,1.40379912232059,2.97219618430927));
#4575=CARTESIAN_POINT('Ctrl Pts',(3.96265200893647,1.43800116895935,3.04847820183902));
#4576=CARTESIAN_POINT('Ctrl Pts',(3.97255653176305,1.48831473982964,3.19024780674964));
#4577=CARTESIAN_POINT('Ctrl Pts',(3.97695707524958,1.50661116414811,3.25472924498381));
#4578=CARTESIAN_POINT('Ctrl Pts',(3.98463974755486,1.53066914784216,3.36653822113341));
#4579=CARTESIAN_POINT('Ctrl Pts',(3.98786841186562,1.53851744739748,3.41331832020172));
#4580=CARTESIAN_POINT('Ctrl Pts',(3.99308676380265,1.54754519080994,3.48786243751187));
#4581=CARTESIAN_POINT('Ctrl Pts',(3.9950318376677,1.55013900021883,3.51542669523062));
#4582=CARTESIAN_POINT('Ctrl Pts',(3.99890865359388,1.5537959718898,3.56981652850039));
#4583=CARTESIAN_POINT('Ctrl Pts',(4.0008383074917,1.55490289421904,3.59662950069241));
#4584=CARTESIAN_POINT('Ctrl Pts',(4.0058148796882,1.55595583761273,3.66504128398193));
#4585=CARTESIAN_POINT('Ctrl Pts',(4.00889081730036,1.55492777078369,3.70663136778311));
#4586=CARTESIAN_POINT('Ctrl Pts',(4.02021507583115,1.5451581658646,3.85717591500451));
#4587=CARTESIAN_POINT('Ctrl Pts',(4.02872846159367,1.52661002056276,3.96516491297887));
#4588=CARTESIAN_POINT('Ctrl Pts',(4.0416298553189,1.4812328812758,4.12578027454465));
#4589=CARTESIAN_POINT('Ctrl Pts',(4.04605113103239,1.46248512658162,4.18035078001407));
#4590=CARTESIAN_POINT('Ctrl Pts',(4.05178295040139,1.43346189450557,4.25166337019466));
#4591=CARTESIAN_POINT('Ctrl Pts',(4.05320695329046,1.42584152590384,4.26943140330701));
#4592=CARTESIAN_POINT('Ctrl Pts',(4.05569830103502,1.4117442759695,4.30067986094914));
#4593=CARTESIAN_POINT('Ctrl Pts',(4.05677251003104,1.40540142053741,4.31421572277039));
#4594=CARTESIAN_POINT('Ctrl Pts',(4.05941129017011,1.38916956655271,4.34759409175537));
#4595=CARTESIAN_POINT('Ctrl Pts',(4.06096245831637,1.37904990282173,4.3673202275207));
#4596=CARTESIAN_POINT('Ctrl Pts',(4.06771803553348,1.33258346637705,4.45331867323967));
#4597=CARTESIAN_POINT('Ctrl Pts',(4.07271401779842,1.29185274847035,4.51711374837032));
#4598=CARTESIAN_POINT('Ctrl Pts',(4.08240829927575,1.20385374876517,4.63503528730301));
#4599=CARTESIAN_POINT('Ctrl Pts',(4.08709734636856,1.15716490630705,4.68934792617514));
#4600=CARTESIAN_POINT('Ctrl Pts',(4.09428522760558,1.08186035945405,4.76562036350551));
#4601=CARTESIAN_POINT('Ctrl Pts',(4.09669956078721,1.05595219040481,4.79011739420133));
#4602=CARTESIAN_POINT('Ctrl Pts',(4.10133405586615,1.0053685171172,4.83475578174971));
#4603=CARTESIAN_POINT('Ctrl Pts',(4.10354607254252,0.980871428792938,4.85507146753235));
#4604=CARTESIAN_POINT('Ctrl Pts',(4.10761129536024,0.935369985281612,4.89050822931019));
#4605=CARTESIAN_POINT('Ctrl Pts',(4.1094534041472,0.914578126148205,4.90588385487765));
#4606=CARTESIAN_POINT('Ctrl Pts',(4.11364728350535,0.86692424435567,4.93931928796557));
#4607=CARTESIAN_POINT('Ctrl Pts',(4.11600971701674,0.839863119069872,4.95707268674783));
#4608=CARTESIAN_POINT('Ctrl Pts',(4.12776720776442,0.704269964340975,5.04009727419388));
#4609=CARTESIAN_POINT('Ctrl Pts',(4.13760696901566,0.58861472270949,5.09277969498722));
#4610=CARTESIAN_POINT('Ctrl Pts',(4.15209204024162,0.410052301754927,5.14909841878641));
#4611=CARTESIAN_POINT('Ctrl Pts',(4.15675058905871,0.351195803164859,5.16394339408211));
#4612=CARTESIAN_POINT('Ctrl Pts',(4.16272218540384,0.272443798948657,5.17897392928248));
#4613=CARTESIAN_POINT('Ctrl Pts',(4.16416081350884,0.253201732900082,5.18227239520491));
#4614=CARTESIAN_POINT('Ctrl Pts',(4.16666552363156,0.219141589904864,5.18745294356212));
#4615=CARTESIAN_POINT('Ctrl Pts',(4.16773886117159,0.204350985223939,5.18948520955101));
#4616=CARTESIAN_POINT('Ctrl Pts',(4.17035850698454,0.167793747187004,5.19397300024505));
#4617=CARTESIAN_POINT('Ctrl Pts',(4.17189195897003,0.146000645682124,5.19618232992628));
#4618=CARTESIAN_POINT('Ctrl Pts',(4.18062243716554,0.0201587373252086,5.20625972862681));
#4619=CARTESIAN_POINT('Ctrl Pts',(4.18740359634422,-0.0844369124588652,
5.20410360241846));
#4620=CARTESIAN_POINT('Ctrl Pts',(4.19917557832368,-0.261661543952743,5.18252119934615));
#4621=CARTESIAN_POINT('Ctrl Pts',(4.2040987530863,-0.334540989733271,5.1683025951143));
#4622=CARTESIAN_POINT('Ctrl Pts',(4.21147563304062,-0.438580618065651,5.14016296928556));
#4623=CARTESIAN_POINT('Ctrl Pts',(4.21380525218518,-0.470741964500488,5.13033494943032));
#4624=CARTESIAN_POINT('Ctrl Pts',(4.21799003989885,-0.527071454822542,5.11110444380182));
#4625=CARTESIAN_POINT('Ctrl Pts',(4.21983064183914,-0.551370894405368,5.10212509645781));
#4626=CARTESIAN_POINT('Ctrl Pts',(4.22390400242872,-0.604033807235253,5.08115563162041));
#4627=CARTESIAN_POINT('Ctrl Pts',(4.22614440236696,-0.632287646929261,5.06892181386123));
#4628=CARTESIAN_POINT('Ctrl Pts',(4.23812145992241,-0.779459349230403,4.99994128604649));
#4629=CARTESIAN_POINT('Ctrl Pts',(4.24835666459985,-0.891152971317602,4.92910139579836));
#4630=CARTESIAN_POINT('Ctrl Pts',(4.2632016428346,-1.03891283267353,4.80664626364936));
#4631=CARTESIAN_POINT('Ctrl Pts',(4.26782534952745,-1.08300182460265,4.76556847845416));
#4632=CARTESIAN_POINT('Ctrl Pts',(4.2737618948435,-1.13806943313479,4.70794065377742));
#4633=CARTESIAN_POINT('Ctrl Pts',(4.27519850063879,-1.15127156698492,4.69359431729355));
#4634=CARTESIAN_POINT('Ctrl Pts',(4.27770133638681,-1.17410413686269,4.667827065502));
#4635=CARTESIAN_POINT('Ctrl Pts',(4.27877476820538,-1.18384496852476,4.65651008880306));
#4636=CARTESIAN_POINT('Ctrl Pts',(4.28114087800316,-1.2051827631869,4.63098531790359));
#4637=CARTESIAN_POINT('Ctrl Pts',(4.28242797244066,-1.21669392899853,4.61670990418397));
#4638=CARTESIAN_POINT('Ctrl Pts',(4.2908026717144,-1.29072584311949,4.52150271466698));
#4639=CARTESIAN_POINT('Ctrl Pts',(4.29746748967359,-1.345395616747,4.43476660068686));
#4640=CARTESIAN_POINT('Ctrl Pts',(4.30949517736764,-1.42707242919977,4.27148493600978));
#4641=CARTESIAN_POINT('Ctrl Pts',(4.31481006451829,-1.45737082104822,4.19702433963268));
#4642=CARTESIAN_POINT('Ctrl Pts',(4.32259461685936,-1.4919546781145,4.08872067062042));
#4643=CARTESIAN_POINT('Ctrl Pts',(4.32491140714319,-1.50109295279396,4.05656098880324));
#4644=CARTESIAN_POINT('Ctrl Pts',(4.32908270041734,-1.51545879030477,3.99901259731048));
#4645=CARTESIAN_POINT('Ctrl Pts',(4.33092301439652,-1.52110124708773,3.97374014819923));
#4646=CARTESIAN_POINT('Ctrl Pts',(4.33500692163564,-1.53209368873157,3.91799691542913));
#4647=CARTESIAN_POINT('Ctrl Pts',(4.33725843599312,-1.53717057127464,3.88748431756645));
#4648=CARTESIAN_POINT('Ctrl Pts',(4.34470269924416,-1.55076865302059,3.78741568145514));
#4649=CARTESIAN_POINT('Ctrl Pts',(4.35000710688228,-1.55550000000259,3.71744083094465));
#4650=CARTESIAN_POINT('Ctrl Pts',(4.35539415465377,-1.5555,3.64739446822634));
#4651=CARTESIAN_POINT('Origin',(1.2059437743963,0.,3.64739446828387));
#4652=CARTESIAN_POINT('',(5.19405622556279,-1.55549955406273,3.6485723098073));
#4653=CARTESIAN_POINT('',(5.05594377443823,-1.5554999873946,3.64759249708933));
#4654=CARTESIAN_POINT('',(1.2059437743963,-1.5555,3.64739446828386));
#4655=CARTESIAN_POINT('Ctrl Pts',(4.49405622566528,-1.55549997006787,3.64769962209176));
#4656=CARTESIAN_POINT('Ctrl Pts',(4.49818264884198,-1.5555112048523,3.59043110243973));
#4657=CARTESIAN_POINT('Ctrl Pts',(4.50230907201867,-1.55235548796177,3.53303695693617));
#4658=CARTESIAN_POINT('Ctrl Pts',(4.50643549519536,-1.54601728863954,3.47589871548614));
#4659=CARTESIAN_POINT('Ctrl Pts',(4.51055471403468,-1.53969015520277,3.41886023190159));
#4660=CARTESIAN_POINT('Ctrl Pts',(4.514673932874,-1.53019162173892,3.36207728507756));
#4661=CARTESIAN_POINT('Ctrl Pts',(4.51879315171332,-1.5175581507441,3.3059306940557));
#4662=CARTESIAN_POINT('Ctrl Pts',(4.52290838596156,-1.50493690032262,3.24983841459506));
#4663=CARTESIAN_POINT('Ctrl Pts',(4.52702362020979,-1.48918683358188,3.1943817831957));
#4664=CARTESIAN_POINT('Ctrl Pts',(4.53113885445802,-1.47039588386744,3.13993393316247));
#4665=CARTESIAN_POINT('Ctrl Pts',(4.53525173244782,-1.45161569328144,3.0855172583184));
#4666=CARTESIAN_POINT('Ctrl Pts',(4.53936461043761,-1.42979824176697,3.0321087172434));
#4667=CARTESIAN_POINT('Ctrl Pts',(4.5434774884274,-1.40508135768999,2.98006649174457));
#4668=CARTESIAN_POINT('Ctrl Pts',(4.54758963497004,-1.38036886934142,2.92803352159878));
#4669=CARTESIAN_POINT('Ctrl Pts',(4.55170178151268,-1.35275819858068,2.87736686006037));
#4670=CARTESIAN_POINT('Ctrl Pts',(4.55581392805532,-1.32243444548001,2.82840277882177));
#4671=CARTESIAN_POINT('Ctrl Pts',(4.55992988829277,-1.2920825694662,2.77939328722124));
#4672=CARTESIAN_POINT('Ctrl Pts',(4.56404584853023,-1.25901286363784,2.73208997848163));
#4673=CARTESIAN_POINT('Ctrl Pts',(4.56816180876768,-1.22345458874825,2.68680136021426));
#4674=CARTESIAN_POINT('Ctrl Pts',(4.5722797249649,-1.18787941608731,2.64149122018524));
#4675=CARTESIAN_POINT('Ctrl Pts',(4.57639764116213,-1.14981366757698,2.59819807345484));
#4676=CARTESIAN_POINT('Ctrl Pts',(4.58051555735935,-1.10952573337367,2.55719590977188));
#4677=CARTESIAN_POINT('Ctrl Pts',(4.58464111268066,-1.06916306124124,2.51611768319655));
#4678=CARTESIAN_POINT('Ctrl Pts',(4.58876666800197,-1.02657036213306,2.47733928112313));
#4679=CARTESIAN_POINT('Ctrl Pts',(4.59289222332329,-0.9820506777324,2.44109570082809));
#4680=CARTESIAN_POINT('Ctrl Pts',(4.59576290545572,-0.95107257839864,2.41587635694221));
#4681=CARTESIAN_POINT('Ctrl Pts',(4.59863358758815,-0.919162176237036,2.39188346783216));
#4682=CARTESIAN_POINT('Ctrl Pts',(4.60150426972059,-0.886429325065602,2.36918349130717));
#4683=CARTESIAN_POINT('Ctrl Pts',(4.60565268890353,-0.839127122506235,2.33637978343416));
#4684=CARTESIAN_POINT('Ctrl Pts',(4.60980110808647,-0.789902466076869,2.30613665572479));
#4685=CARTESIAN_POINT('Ctrl Pts',(4.61394952726942,-0.739063605726851,2.27868513585056));
#4686=CARTESIAN_POINT('Ctrl Pts',(4.61809058315377,-0.688314982571362,2.25128234146157));
#4687=CARTESIAN_POINT('Ctrl Pts',(4.62223163903812,-0.63595829684667,2.22666156523234));
#4688=CARTESIAN_POINT('Ctrl Pts',(4.62637269492247,-0.582330668195458,2.20501059327728));
#4689=CARTESIAN_POINT('Ctrl Pts',(4.6305096393609,-0.528756283716943,2.18338111748229));
#4690=CARTESIAN_POINT('Ctrl Pts',(4.63464658379934,-0.473913936833424,2.16471579788024));
#4691=CARTESIAN_POINT('Ctrl Pts',(4.63878352823778,-0.418163666519841,2.14915570293214));
#4692=CARTESIAN_POINT('Ctrl Pts',(4.64291795482279,-0.362447327290285,2.13360507826797));
#4693=CARTESIAN_POINT('Ctrl Pts',(4.64705238140779,-0.305824660527237,2.12115607155639));
#4694=CARTESIAN_POINT('Ctrl Pts',(4.6511868079928,-0.248671830850126,2.11190022520067));
#4695=CARTESIAN_POINT('Ctrl Pts',(4.65532030671694,-0.191531827588675,2.10264645607075));
#4696=CARTESIAN_POINT('Ctrl Pts',(4.65945380544109,-0.133862411372917,2.09658450778816));
#4697=CARTESIAN_POINT('Ctrl Pts',(4.66358730416523,-0.0760487419178204,
2.09375460047257));
#4698=CARTESIAN_POINT('Ctrl Pts',(4.66772453540496,-0.0181828671914085,
2.09092213777379));
#4699=CARTESIAN_POINT('Ctrl Pts',(4.67186176664469,0.0398269998097328,2.09132757497707));
#4700=CARTESIAN_POINT('Ctrl Pts',(4.67599899788442,0.0975931575226902,2.09495901854538));
#4701=CARTESIAN_POINT('Ctrl Pts',(4.68013794257913,0.155383239378352,2.09859196609417));
#4702=CARTESIAN_POINT('Ctrl Pts',(4.68427688727384,0.21292889243015,2.10545352302033));
#4703=CARTESIAN_POINT('Ctrl Pts',(4.68841583196855,0.269848249449869,2.1154799235821));
#4704=CARTESIAN_POINT('Ctrl Pts',(4.69256282156823,0.326878241148732,2.1255258125511));
#4705=CARTESIAN_POINT('Ctrl Pts',(4.69670981116791,0.383278995100267,2.13874871992924));
#4706=CARTESIAN_POINT('Ctrl Pts',(4.7008568007676,0.438680449723801,2.15503401818137));
#4707=CARTESIAN_POINT('Ctrl Pts',(4.70474847060895,0.490670975608444,2.17031667142703));
#4708=CARTESIAN_POINT('Ctrl Pts',(4.70864014045031,0.541781273715245,2.18829563175242));
#4709=CARTESIAN_POINT('Ctrl Pts',(4.71253181029166,0.59172248829761,2.20883798804304));
#4710=CARTESIAN_POINT('Ctrl Pts',(4.71668022643349,0.644958489593126,2.23073559136017));
#4711=CARTESIAN_POINT('Ctrl Pts',(4.72082864257532,0.697088813768266,2.25563816533532));
#4712=CARTESIAN_POINT('Ctrl Pts',(4.72497705871715,0.747752051956174,2.28341238673172));
#4713=CARTESIAN_POINT('Ctrl Pts',(4.7291181115616,0.798325364621586,2.31113730983097));
#4714=CARTESIAN_POINT('Ctrl Pts',(4.73325916440605,0.84743630712596,2.34172351508062));
#4715=CARTESIAN_POINT('Ctrl Pts',(4.7374002172505,0.894744095649229,2.3749899519052));
#4716=CARTESIAN_POINT('Ctrl Pts',(4.74153715865178,0.942004914647769,2.40822336015719));
#4717=CARTESIAN_POINT('Ctrl Pts',(4.74567410005306,0.987465702944323,2.44413142958443));
#4718=CARTESIAN_POINT('Ctrl Pts',(4.74981104145434,1.0308124524694,2.4824884901749));
#4719=CARTESIAN_POINT('Ctrl Pts',(4.75394546500998,1.07413282008236,2.5208222057023));
#4720=CARTESIAN_POINT('Ctrl Pts',(4.75807988856561,1.11534131031358,2.56160161338362));
#4721=CARTESIAN_POINT('Ctrl Pts',(4.76221431212125,1.1541567390143,2.60456060242226));
#4722=CARTESIAN_POINT('Ctrl Pts',(4.76634780782885,1.19296345674993,2.64750995059728));
#4723=CARTESIAN_POINT('Ctrl Pts',(4.77048130353644,1.22937783025481,2.69263752287338));
#4724=CARTESIAN_POINT('Ctrl Pts',(4.77461479924404,1.26315688060035,2.73964177895049));
#4725=CARTESIAN_POINT('Ctrl Pts',(4.77875202751133,1.29696643353513,2.78668848001941));
#4726=CARTESIAN_POINT('Ctrl Pts',(4.78288925577862,1.32813560223623,2.83561482825154));
#4727=CARTESIAN_POINT('Ctrl Pts',(4.78702648404591,1.35646378270176,2.88608884225813));
#4728=CARTESIAN_POINT('Ctrl Pts',(4.79116542578736,1.38480369556448,2.93658376057877));
#4729=CARTESIAN_POINT('Ctrl Pts',(4.79530436752881,1.41030004380517,2.98862715446279));
#4730=CARTESIAN_POINT('Ctrl Pts',(4.79944330927026,1.43279894537414,3.04186376540024));
#4731=CARTESIAN_POINT('Ctrl Pts',(4.8035902959877,1.4553415786828,3.09520385381655));
#4732=CARTESIAN_POINT('Ctrl Pts',(4.80773728270514,1.47487494518795,3.14974130245457));
#4733=CARTESIAN_POINT('Ctrl Pts',(4.81188426942258,1.49129427990581,3.20510313814026));
#4734=CARTESIAN_POINT('Ctrl Pts',(4.81577596323597,1.50670282295052,3.25705684045857));
#4735=CARTESIAN_POINT('Ctrl Pts',(4.81966765704935,1.51936934366868,3.30973606651607));
#4736=CARTESIAN_POINT('Ctrl Pts',(4.82355935086274,1.529248536561,3.36282608735225));
#4737=CARTESIAN_POINT('Ctrl Pts',(4.82770776987243,1.53977943481765,3.41941832256454));
#4738=CARTESIAN_POINT('Ctrl Pts',(4.83185618888211,1.54718672201663,3.47671443938878));
#4739=CARTESIAN_POINT('Ctrl Pts',(4.8360046078918,1.55138603020247,3.53433857373336));
#4740=CARTESIAN_POINT('Ctrl Pts',(4.84014566356742,1.5555778847273,3.59186042676296));
#4741=CARTESIAN_POINT('Ctrl Pts',(4.84428671924304,1.55657302470185,3.64970862663667));
#4742=CARTESIAN_POINT('Ctrl Pts',(4.84842777491866,1.55433835797629,3.7074987021079));
#4743=CARTESIAN_POINT('Ctrl Pts',(4.85256471912704,1.55210590995044,3.76523140042202));
#4744=CARTESIAN_POINT('Ctrl Pts',(4.85670166333542,1.54665002876786,3.82290557099121));
#4745=CARTESIAN_POINT('Ctrl Pts',(4.8608386075438,1.53798962954334,3.88013498778392));
#4746=CARTESIAN_POINT('Ctrl Pts',(4.86497303387806,1.52933450130966,3.93732957295696));
#4747=CARTESIAN_POINT('Ctrl Pts',(4.86910746021232,1.51747879900517,3.99407942716112));
#4748=CARTESIAN_POINT('Ctrl Pts',(4.87324188654659,1.50249322175681,4.0500039174711));
#4749=CARTESIAN_POINT('Ctrl Pts',(4.87737538499991,1.48751100769124,4.10591585676085));
#4750=CARTESIAN_POINT('Ctrl Pts',(4.88150888345323,1.46940044792973,4.16100229719957));
#4751=CARTESIAN_POINT('Ctrl Pts',(4.88564238190656,1.44828274104247,4.21489543920685));
#4752=CARTESIAN_POINT('Ctrl Pts',(4.88977961284657,1.42714596518473,4.26883724590764));
#4753=CARTESIAN_POINT('Ctrl Pts',(4.89391684378659,1.40299680515486,4.32158311447311));
#4754=CARTESIAN_POINT('Ctrl Pts',(4.89805407472661,1.37600503548618,4.37278428921926));
#4755=CARTESIAN_POINT('Ctrl Pts',(4.90219301910532,1.34900208714669,4.4240066689877));
#4756=CARTESIAN_POINT('Ctrl Pts',(4.90633196348404,1.31915444986936,4.47368263163854));
#4757=CARTESIAN_POINT('Ctrl Pts',(4.91047090786276,1.28667682036269,4.52149000650688));
#4758=CARTESIAN_POINT('Ctrl Pts',(4.9146178971234,1.25413606396402,4.56939030475157));
#4759=CARTESIAN_POINT('Ctrl Pts',(4.91876488638405,1.21895541635315,4.61541434136031));
#4760=CARTESIAN_POINT('Ctrl Pts',(4.9229118756447,1.18139112703999,4.6592715630692));
#4761=CARTESIAN_POINT('Ctrl Pts',(4.9268035475744,1.14613955509435,4.70042863098328));
#4762=CARTESIAN_POINT('Ctrl Pts',(4.93069521950411,1.10878944216813,4.73967755409276));
#4763=CARTESIAN_POINT('Ctrl Pts',(4.93458689143382,1.06958042727821,4.77680934315641));
#4764=CARTESIAN_POINT('Ctrl Pts',(4.93873531572807,1.02778460459304,4.81639089541027));
#4765=CARTESIAN_POINT('Ctrl Pts',(4.94288374002232,0.983701114049866,4.85373212912805));
#4766=CARTESIAN_POINT('Ctrl Pts',(4.94703216431657,0.937599712680949,4.88855804685867));
#4767=CARTESIAN_POINT('Ctrl Pts',(4.95117322534675,0.89158013919844,4.92332215017247));
#4768=CARTESIAN_POINT('Ctrl Pts',(4.95531428637694,0.843550176143952,4.95557948781594));
#4769=CARTESIAN_POINT('Ctrl Pts',(4.95945534740713,0.793814658995242,4.98509343933987));
#4770=CARTESIAN_POINT('Ctrl Pts',(4.96359229700889,0.744128521466237,5.01457808810822));
#4771=CARTESIAN_POINT('Ctrl Pts',(4.96772924661065,0.692740630421661,5.04132448297694));
#4772=CARTESIAN_POINT('Ctrl Pts',(4.97186619621242,0.639985543720192,5.06513871666902));
#4773=CARTESIAN_POINT('Ctrl Pts',(4.97600062796938,0.587262565004926,5.08893845645853));
#4774=CARTESIAN_POINT('Ctrl Pts',(4.98013505972634,0.53317451373346,5.10980935885719));
#4775=CARTESIAN_POINT('Ctrl Pts',(4.98426949148331,0.478079379464018,5.12760403349121));
#4776=CARTESIAN_POINT('Ctrl Pts',(4.98840299537921,0.422996609803011,5.14539471459318));
#4777=CARTESIAN_POINT('Ctrl Pts',(4.99253649927511,0.366907701096048,5.16011037858374));
#4778=CARTESIAN_POINT('Ctrl Pts',(4.99667000317101,0.310187297829131,5.17165300615252));
#4779=CARTESIAN_POINT('Ctrl Pts',(5.00080723954057,0.253415677140779,5.18320605648958));
#4780=CARTESIAN_POINT('Ctrl Pts',(5.00494447591013,0.196011933603237,5.19158023947205));
#4781=CARTESIAN_POINT('Ctrl Pts',(5.00908171227969,0.138361107359043,5.19672866527637));
#4782=CARTESIAN_POINT('Ctrl Pts',(5.01322066208979,0.0806864049679458,5.20187922330634));
#4783=CARTESIAN_POINT('Ctrl Pts',(5.0173596118999,0.0227649373575623,5.20380134227935));
#4784=CARTESIAN_POINT('Ctrl Pts',(5.02149856171001,-0.0350161759652235,
5.20250029022036));
#4785=CARTESIAN_POINT('Ctrl Pts',(5.02564555633343,-0.0929095975523984,
5.20119670932643));
#4786=CARTESIAN_POINT('Ctrl Pts',(5.02979255095684,-0.150661598631284,5.19665747786722));
#4787=CARTESIAN_POINT('Ctrl Pts',(5.03393954558026,-0.207889035771002,5.18893992619493));
#4788=CARTESIAN_POINT('Ctrl Pts',(5.03783117438847,-0.261592491699183,5.18169760997701));
#4789=CARTESIAN_POINT('Ctrl Pts',(5.04172280319669,-0.31483371984599,5.17165692314211));
#4790=CARTESIAN_POINT('Ctrl Pts',(5.0456144320049,-0.367307093263548,5.15890554969819));
#4791=CARTESIAN_POINT('Ctrl Pts',(5.04976283477336,-0.423242717724022,5.14531282657291));
#4792=CARTESIAN_POINT('Ctrl Pts',(5.05391123754182,-0.478539950070369,5.12858247703885));
#4793=CARTESIAN_POINT('Ctrl Pts',(5.05805964031028,-0.532821374525066,5.10879161924908));
#4794=CARTESIAN_POINT('Ctrl Pts',(5.06220067980811,-0.587006451339394,5.08903588954351));
#4795=CARTESIAN_POINT('Ctrl Pts',(5.06634171930595,-0.640178813856002,5.06623061086352));
#4796=CARTESIAN_POINT('Ctrl Pts',(5.07048275880378,-0.69197421424734,5.04050319943761));
#4797=CARTESIAN_POINT('Ctrl Pts',(5.07461968688348,-0.743718189737107,5.01480133139181));
#4798=CARTESIAN_POINT('Ctrl Pts',(5.07875661496318,-0.794087447787288,4.98618330930369));
#4799=CARTESIAN_POINT('Ctrl Pts',(5.08289354304288,-0.842737458631716,4.95482470574167));
#4800=CARTESIAN_POINT('Ctrl Pts',(5.08702795332396,-0.891357860324755,4.92348518751229));
#4801=CARTESIAN_POINT('Ctrl Pts',(5.09116236360505,-0.938260652246804,4.88940867573679));
#4802=CARTESIAN_POINT('Ctrl Pts',(5.09529677388614,-0.983127633410414,4.85281568363759));
#4803=CARTESIAN_POINT('Ctrl Pts',(5.09943025638825,-1.0279845462356,4.81623090315903));
#4804=CARTESIAN_POINT('Ctrl Pts',(5.10356373889036,-1.07080615196526,4.77713109241526));
#4805=CARTESIAN_POINT('Ctrl Pts',(5.10769722139246,-1.11130665585478,4.73577756565945));
#4806=CARTESIAN_POINT('Ctrl Pts',(5.11183443666738,-1.15184373403227,4.69438669428688));
#4807=CARTESIAN_POINT('Ctrl Pts',(5.11597165194229,-1.19005515556612,4.65073841184166));
#4808=CARTESIAN_POINT('Ctrl Pts',(5.1201088672172,-1.22569240828007,4.60513053332716));
#4809=CARTESIAN_POINT('Ctrl Pts',(5.12424779606124,-1.26134442138042,4.55950376475076));
#4810=CARTESIAN_POINT('Ctrl Pts',(5.12838672490527,-1.29441984130356,4.51191620982779));
#4811=CARTESIAN_POINT('Ctrl Pts',(5.13252565374931,-1.32471281917244,4.46269576027366));
#4812=CARTESIAN_POINT('Ctrl Pts',(5.1366726278983,-1.35506468093469,4.41337963535488));
#4813=CARTESIAN_POINT('Ctrl Pts',(5.14081960204729,-1.38262304284483,4.36242473206691));
#4814=CARTESIAN_POINT('Ctrl Pts',(5.14496657619628,-1.4072279282867,4.31018388269083));
#4815=CARTESIAN_POINT('Ctrl Pts',(5.14885837498951,-1.43031880371297,4.26115756440314));
#4816=CARTESIAN_POINT('Ctrl Pts',(5.15275017378274,-1.45080881805192,4.21099922990181));
#4817=CARTESIAN_POINT('Ctrl Pts',(5.15664197257597,-1.46860557248654,4.16001315938037));
#4818=CARTESIAN_POINT('Ctrl Pts',(5.16149448951435,-1.49079558202462,4.09644081559507));
#4819=CARTESIAN_POINT('Ctrl Pts',(5.16634700645272,-1.50887543297736,4.03136398579808));
#4820=CARTESIAN_POINT('Ctrl Pts',(5.1711995233911,-1.52267165228913,3.96528012274959));
#4821=CARTESIAN_POINT('Ctrl Pts',(5.17600347704233,-1.53632980103497,3.89985761743711));
#4822=CARTESIAN_POINT('Ctrl Pts',(5.18080743069357,-1.54578953856301,3.83344827699785));
#4823=CARTESIAN_POINT('Ctrl Pts',(5.18561138434481,-1.55092904889536,3.76655543207882));
#4824=CARTESIAN_POINT('Ctrl Pts',(5.18842633141747,-1.55394062032491,3.72735858888317));
#4825=CARTESIAN_POINT('Ctrl Pts',(5.19124127849013,-1.55546970192271,3.6879961113706));
#4826=CARTESIAN_POINT('Ctrl Pts',(5.19405622556279,-1.55549955406273,3.64857230980729));
#4827=CARTESIAN_POINT('Ctrl Pts',(4.35539415465377,-1.5555,3.64739446822634));
#4828=CARTESIAN_POINT('Ctrl Pts',(4.35542999814836,-1.55549999999998,3.64692840471077));
#4829=CARTESIAN_POINT('Ctrl Pts',(4.35546584504022,-1.55549979055614,3.64646233800919));
#4830=CARTESIAN_POINT('Ctrl Pts',(4.36188857679378,-1.55542473595912,3.56296395502291));
#4831=CARTESIAN_POINT('Ctrl Pts',(4.3683744954262,-1.54870199287245,3.48007311827889));
#4832=CARTESIAN_POINT('Ctrl Pts',(4.37785809760788,-1.52889270440881,3.35806064973541));
#4833=CARTESIAN_POINT('Ctrl Pts',(4.38093859904207,-1.52082399216784,3.31827147924459));
#4834=CARTESIAN_POINT('Ctrl Pts',(4.38531873479868,-1.50684734298434,3.2609621066012));
#4835=CARTESIAN_POINT('Ctrl Pts',(4.3866710431493,-1.50217004120609,3.24316169155456));
#4836=CARTESIAN_POINT('Ctrl Pts',(4.38910145249918,-1.49307977307113,3.21090706305394));
#4837=CARTESIAN_POINT('Ctrl Pts',(4.39018445434306,-1.48877062776986,3.19642827795493));
#4838=CARTESIAN_POINT('Ctrl Pts',(4.39294051384069,-1.47714668947666,3.15935583138246));
#4839=CARTESIAN_POINT('Ctrl Pts',(4.3945968999736,-1.46952431871857,3.13686289014797));
#4840=CARTESIAN_POINT('Ctrl Pts',(4.3983386853491,-1.45091238522659,3.08581728243223));
#4841=CARTESIAN_POINT('Ctrl Pts',(4.40040948261443,-1.43958953000532,3.05739624327089));
#4842=CARTESIAN_POINT('Ctrl Pts',(4.40816645041642,-1.39359871348182,2.95118001327666));
#4843=CARTESIAN_POINT('Ctrl Pts',(4.41370528325849,-1.3534009877825,2.87594199554479));
#4844=CARTESIAN_POINT('Ctrl Pts',(4.42377475954006,-1.27096408468807,2.7481102953198));
#4845=CARTESIAN_POINT('Ctrl Pts',(4.42825545667103,-1.23109277752972,2.69425711502341));
#4846=CARTESIAN_POINT('Ctrl Pts',(4.43498426132566,-1.16800436737407,2.61963291254183));
#4847=CARTESIAN_POINT('Ctrl Pts',(4.43712901503915,-1.14743635971122,2.59671964265138));
#4848=CARTESIAN_POINT('Ctrl Pts',(4.44113146877616,-1.10833588627031,2.55567895097272));
#4849=CARTESIAN_POINT('Ctrl Pts',(4.44298009405443,-1.09000387279486,2.53737527190498));
#4850=CARTESIAN_POINT('Ctrl Pts',(4.4472756489092,-1.04684672837059,2.49638511099431));
#4851=CARTESIAN_POINT('Ctrl Pts',(4.44973562529083,-1.02172668075679,2.47402970038334));
#4852=CARTESIAN_POINT('Ctrl Pts',(4.45772661735186,-0.938928703210286,2.40501999259118));
#4853=CARTESIAN_POINT('Ctrl Pts',(4.46337778056004,-0.878637787054404,2.36167507033744));
#4854=CARTESIAN_POINT('Ctrl Pts',(4.47715923622267,-0.726626581277186,2.26808858605382));
#4855=CARTESIAN_POINT('Ctrl Pts',(4.48533743175627,-0.632476451274925,2.22245708528392));
#4856=CARTESIAN_POINT('Ctrl Pts',(4.49479424411113,-0.513896047406532,2.17907206156494));
#4857=CARTESIAN_POINT('Ctrl Pts',(4.49641661501248,-0.493171773749606,2.17198212850311));
#4858=CARTESIAN_POINT('Ctrl Pts',(4.49910532165137,-0.458079326012556,2.16079887788346));
#4859=CARTESIAN_POINT('Ctrl Pts',(4.50018369446635,-0.443790664739438,2.1564709188448));
#4860=CARTESIAN_POINT('Ctrl Pts',(4.50264447935619,-0.41067826895064,2.14695964673776));
#4861=CARTESIAN_POINT('Ctrl Pts',(4.50401897428641,-0.391815574230527,2.14192379497556));
#4862=CARTESIAN_POINT('Ctrl Pts',(4.50959855783353,-0.313977050032548,2.12270516721578));
#4863=CARTESIAN_POINT('Ctrl Pts',(4.51366228573272,-0.25428516122497,2.11162111071013));
#4864=CARTESIAN_POINT('Ctrl Pts',(4.52606993601889,-0.0684829468292242,
2.08825446455552));
#4865=CARTESIAN_POINT('Ctrl Pts',(4.53425766468571,0.0585741758225829,2.08785139797019));
#4866=CARTESIAN_POINT('Ctrl Pts',(4.5451646093482,0.216408854517286,2.10668202767637));
#4867=CARTESIAN_POINT('Ctrl Pts',(4.54741203071619,0.24841434475502,2.11151762772885));
#4868=CARTESIAN_POINT('Ctrl Pts',(4.55151215067338,0.305677513143337,2.12200596710734));
#4869=CARTESIAN_POINT('Ctrl Pts',(4.55335270308443,0.330989559565052,2.12729756806459));
#4870=CARTESIAN_POINT('Ctrl Pts',(4.5575039691887,0.387127098001942,2.14050193863269));
#4871=CARTESIAN_POINT('Ctrl Pts',(4.55982431334069,0.417864477660873,2.14873457099207));
#4872=CARTESIAN_POINT('Ctrl Pts',(4.56922601848365,0.539747479762893,2.18542045337305));
#4873=CARTESIAN_POINT('Ctrl Pts',(4.57653994180552,0.628426750286668,2.22129153993351));
#4874=CARTESIAN_POINT('Ctrl Pts',(4.59078706731346,0.791868255272748,2.30562245244562));
#4875=CARTESIAN_POINT('Ctrl Pts',(4.597679539285,0.866892415079856,2.35282605929805));
#4876=CARTESIAN_POINT('Ctrl Pts',(4.60592319943792,0.954771650292071,2.41920075137131));
#4877=CARTESIAN_POINT('Ctrl Pts',(4.6075258349408,0.97176988712405,2.43260554580481));
#4878=CARTESIAN_POINT('Ctrl Pts',(4.6101937199705,0.999998791079666,2.45583873107124));
#4879=CARTESIAN_POINT('Ctrl Pts',(4.61127050077445,1.01137685470935,2.46548094434886));
#4880=CARTESIAN_POINT('Ctrl Pts',(4.613742968741,1.03747024495647,2.4882463572274));
#4881=CARTESIAN_POINT('Ctrl Pts',(4.61513033147309,1.05207774628456,2.50148811569253));
#4882=CARTESIAN_POINT('Ctrl Pts',(4.62097017138366,1.11320178934594,2.55905182138824));
#4883=CARTESIAN_POINT('Ctrl Pts',(4.62526321254511,1.15720499907292,2.6059596510751));
#4884=CARTESIAN_POINT('Ctrl Pts',(4.63745006339755,1.27467787353898,2.74785836622972));
#4885=CARTESIAN_POINT('Ctrl Pts',(4.6452288041292,1.34022062815111,2.84878601565727));
#4886=CARTESIAN_POINT('Ctrl Pts',(4.65570114374138,1.40816552533107,2.98577733975348));
#4887=CARTESIAN_POINT('Ctrl Pts',(4.65798652166037,1.42187189399599,3.01577162522033));
#4888=CARTESIAN_POINT('Ctrl Pts',(4.66212562874524,1.44462423359303,3.07006283812805));
#4889=CARTESIAN_POINT('Ctrl Pts',(4.66396610915149,1.4540356366406,3.09419359364092));
#4890=CARTESIAN_POINT('Ctrl Pts',(4.66804353334394,1.47332480837505,3.14754915902081));
#4891=CARTESIAN_POINT('Ctrl Pts',(4.67028822661346,1.48294422274814,3.17685488018609));
#4892=CARTESIAN_POINT('Ctrl Pts',(4.67824178661334,1.51353851851047,3.28034753753506));
#4893=CARTESIAN_POINT('Ctrl Pts',(4.68409277103487,1.52986293152239,3.35578087399551));
#4894=CARTESIAN_POINT('Ctrl Pts',(4.69864160539919,1.55598401909998,3.54269161394477));
#4895=CARTESIAN_POINT('Ctrl Pts',(4.70741080660326,1.55948670067154,3.65462557599081));
#4896=CARTESIAN_POINT('Ctrl Pts',(4.71730637109817,1.54938978687576,3.78668991388579));
#4897=CARTESIAN_POINT('Ctrl Pts',(4.71884206424525,1.54739089558878,3.80737404655244));
#4898=CARTESIAN_POINT('Ctrl Pts',(4.72144090338253,1.5432497279148,3.8427967889763));
#4899=CARTESIAN_POINT('Ctrl Pts',(4.72251385516975,1.54130938448318,3.85755446356819));
#4900=CARTESIAN_POINT('Ctrl Pts',(4.72503404277329,1.5361989712694,3.89253042639371));
#4901=CARTESIAN_POINT('Ctrl Pts',(4.72647139029881,1.53284133217306,3.91271781506562));
#4902=CARTESIAN_POINT('Ctrl Pts',(4.73343568334681,1.51442895415891,4.01135192369608));
#4903=CARTESIAN_POINT('Ctrl Pts',(4.73871374853264,1.49374387002476,4.08863427287779));
#4904=CARTESIAN_POINT('Ctrl Pts',(4.750684797881,1.43339664767971,4.26002840439575));
#4905=CARTESIAN_POINT('Ctrl Pts',(4.75735105332211,1.39023993880161,4.35250204427422));
#4906=CARTESIAN_POINT('Ctrl Pts',(4.76659517836645,1.32141431672016,4.46870457304304));
#4907=CARTESIAN_POINT('Ctrl Pts',(4.76889899232322,1.30355572206415,4.49676381389284));
#4908=CARTESIAN_POINT('Ctrl Pts',(4.77305760987036,1.27020392361317,4.5456337947288));
#4909=CARTESIAN_POINT('Ctrl Pts',(4.77489863236737,1.25506321549494,4.56667030988139));
#4910=CARTESIAN_POINT('Ctrl Pts',(4.77896090515028,1.22089527603014,4.6117249588905));
#4911=CARTESIAN_POINT('Ctrl Pts',(4.78118949796384,1.20167003309675,4.63557838549447));
#4912=CARTESIAN_POINT('Ctrl Pts',(4.78889779482462,1.13362552026516,4.71507977555612));
#4913=CARTESIAN_POINT('Ctrl Pts',(4.79450670797288,1.08155148228075,4.76779718023151));
#4914=CARTESIAN_POINT('Ctrl Pts',(4.80862472208468,0.94372030124631,4.888738261238));
#4915=CARTESIAN_POINT('Ctrl Pts',(4.81721382787897,0.85413091192074,4.95200322046696));
#4916=CARTESIAN_POINT('Ctrl Pts',(4.82721213351643,0.737985491933357,5.01688987330132));
#4917=CARTESIAN_POINT('Ctrl Pts',(4.82897088054911,0.717064268724508,5.02795929747552));
#4918=CARTESIAN_POINT('Ctrl Pts',(4.83180750888367,0.682396168718489,5.0453013342007));
#4919=CARTESIAN_POINT('Ctrl Pts',(4.8329009139097,0.668796918936155,5.05185838695539));
#4920=CARTESIAN_POINT('Ctrl Pts',(4.83530242752549,0.638375372114797,5.06598435427532));
#4921=CARTESIAN_POINT('Ctrl Pts',(4.83660495433967,0.621510239991016,5.07345389440286));
#4922=CARTESIAN_POINT('Ctrl Pts',(4.84118905144667,0.56101894520581,5.09896826849431));
#4923=CARTESIAN_POINT('Ctrl Pts',(4.84438720824956,0.516705411285167,5.11532675360132));
#4924=CARTESIAN_POINT('Ctrl Pts',(4.85446620191945,0.37294074930458,5.16107846928913));
#4925=CARTESIAN_POINT('Ctrl Pts',(4.86116949193477,0.271274634416704,5.18256064697489));
#4926=CARTESIAN_POINT('Ctrl Pts',(4.87159525689092,0.116302225914969,5.19941957635496));
#4927=CARTESIAN_POINT('Ctrl Pts',(4.87513613217272,0.0641326501568996,5.20244889535822));
#4928=CARTESIAN_POINT('Ctrl Pts',(4.88072251576621,-0.0164446018107013,
5.20306604165799));
#4929=CARTESIAN_POINT('Ctrl Pts',(4.88271056757386,-0.0448014086357122,
5.20250768550618));
#4930=CARTESIAN_POINT('Ctrl Pts',(4.88660061734454,-0.0995476006223623,
5.19993116531816));
#4931=CARTESIAN_POINT('Ctrl Pts',(4.88849875925825,-0.125932011716523,5.19801398626185));
#4932=CARTESIAN_POINT('Ctrl Pts',(4.89323784166347,-0.190919086001194,5.1916223202721));
#4933=CARTESIAN_POINT('Ctrl Pts',(4.89610204047956,-0.229425390676273,5.18637245868275));
#4934=CARTESIAN_POINT('Ctrl Pts',(4.90261128007893,-0.315167928486089,5.17139321982818));
#4935=CARTESIAN_POINT('Ctrl Pts',(4.90627528374493,-0.362228767899446,5.16089788706049));
#4936=CARTESIAN_POINT('Ctrl Pts',(4.91631346841617,-0.48828377189565,5.12656943373389));
#4937=CARTESIAN_POINT('Ctrl Pts',(4.92275265020067,-0.565993017195498,5.09861154329901));
#4938=CARTESIAN_POINT('Ctrl Pts',(4.9324802103248,-0.681318222210005,5.04644144098251));
#4939=CARTESIAN_POINT('Ctrl Pts',(4.93583549528687,-0.720729797261556,5.02655227388476));
#4940=CARTESIAN_POINT('Ctrl Pts',(4.94047542075217,-0.775274249858286,4.99604837298498));
#4941=CARTESIAN_POINT('Ctrl Pts',(4.94182485360825,-0.791143832536963,4.98680069427455));
#4942=CARTESIAN_POINT('Ctrl Pts',(4.94425300457878,-0.819770156054677,4.9694329050093));
#4943=CARTESIAN_POINT('Ctrl Pts',(4.94533654303652,-0.832577515460654,4.96140490989313));
#4944=CARTESIAN_POINT('Ctrl Pts',(4.94809827914855,-0.865263047690833,4.94024692315991));
#4945=CARTESIAN_POINT('Ctrl Pts',(4.94975964888325,-0.884960198690081,4.92684482764504));
#4946=CARTESIAN_POINT('Ctrl Pts',(4.95351556659746,-0.929341003110109,4.89513222517167));
#4947=CARTESIAN_POINT('Ctrl Pts',(4.95559534563289,-0.953805791714416,4.87653195418727));
#4948=CARTESIAN_POINT('Ctrl Pts',(4.96342313172155,-1.04466894829505,4.80310194256126));
#4949=CARTESIAN_POINT('Ctrl Pts',(4.96902121029276,-1.10702655824849,4.74351781423349));
#4950=CARTESIAN_POINT('Ctrl Pts',(4.97912162544132,-1.20817945042595,4.62937846219486));
#4951=CARTESIAN_POINT('Ctrl Pts',(4.98356951491534,-1.24899155391738,4.57691519101357));
#4952=CARTESIAN_POINT('Ctrl Pts',(4.99024979490359,-1.30351071678685,4.49673206698423));
#4953=CARTESIAN_POINT('Ctrl Pts',(4.99238028670559,-1.31994736541699,4.47095580374915));
#4954=CARTESIAN_POINT('Ctrl Pts',(4.99637018492174,-1.34890043924445,4.42245564211075));
#4955=CARTESIAN_POINT('Ctrl Pts',(4.99822095401451,-1.36162847951736,4.39987035028918));
#4956=CARTESIAN_POINT('Ctrl Pts',(5.00254252365421,-1.38970350501572,4.34700591126335));
#4957=CARTESIAN_POINT('Ctrl Pts',(5.00502696997582,-1.40463496537909,4.31652247066382));
#4958=CARTESIAN_POINT('Ctrl Pts',(5.01380759801659,-1.45319750922058,4.20857734789363));
#4959=CARTESIAN_POINT('Ctrl Pts',(5.02026927270878,-1.48150659564499,4.1288958746411));
#4960=CARTESIAN_POINT('Ctrl Pts',(5.03432931649413,-1.52821031127595,3.95335084451619));
#4961=CARTESIAN_POINT('Ctrl Pts',(5.04192309163973,-1.54434640482295,3.85723503067018));
#4962=CARTESIAN_POINT('Ctrl Pts',(5.05064964285584,-1.5528331032241,3.74055544888774));
#4963=CARTESIAN_POINT('Ctrl Pts',(5.05210625422466,-1.55389003551992,3.72084835309325));
#4964=CARTESIAN_POINT('Ctrl Pts',(5.05424920512365,-1.5549065266014,3.69143861100837));
#4965=CARTESIAN_POINT('Ctrl Pts',(5.05495023095125,-1.55515079715118,3.68174869778304));
#4966=CARTESIAN_POINT('Ctrl Pts',(5.05622915306735,-1.55543323587685,3.6639366758968));
#4967=CARTESIAN_POINT('Ctrl Pts',(5.05680862740202,-1.55549840327986,3.65581588846268));
#4968=CARTESIAN_POINT('Ctrl Pts',(5.05738485701521,-1.55549997101641,3.64769474805265));
#4969=CARTESIAN_POINT('Origin',(1.2059437743963,0.,3.64739446828387));
#4970=CARTESIAN_POINT('',(5.89405622564623,-1.55549964733824,3.6463470282533));
#4971=CARTESIAN_POINT('',(5.7559437743963,-1.5554995134887,3.64862472695888));
#4972=CARTESIAN_POINT('',(1.2059437743963,-1.5555,3.64739446828386));
#4973=CARTESIAN_POINT('Ctrl Pts',(5.1940562256037,-1.55549955406316,3.6485723092344));
#4974=CARTESIAN_POINT('Ctrl Pts',(5.19818989105023,-1.55554339101516,3.59067963768889));
#4975=CARTESIAN_POINT('Ctrl Pts',(5.20232355649676,-1.55235092862268,3.53275114493701));
#4976=CARTESIAN_POINT('Ctrl Pts',(5.20645722194329,-1.54593674727678,3.47517419241811));
#4977=CARTESIAN_POINT('Ctrl Pts',(5.21059031289217,-1.5395234573751,3.41760524195563));
#4978=CARTESIAN_POINT('Ctrl Pts',(5.21472340384104,-1.52988939577036,3.36038825123365));
#4979=CARTESIAN_POINT('Ctrl Pts',(5.21885649478992,-1.51710097035121,3.30390517331323));
#4980=CARTESIAN_POINT('Ctrl Pts',(5.22299383790471,-1.50429938807019,3.24736398502896));
#4981=CARTESIAN_POINT('Ctrl Pts',(5.22713118101951,-1.48833707342143,3.19155872648217));
#4982=CARTESIAN_POINT('Ctrl Pts',(5.2312685241343,-1.46933126780931,3.13685957678488));
#4983=CARTESIAN_POINT('Ctrl Pts',(5.23540787466692,-1.45031624067703,3.08213388733853));
#4984=CARTESIAN_POINT('Ctrl Pts',(5.23954722519954,-1.4282549783926,3.02851585791735));
#4985=CARTESIAN_POINT('Ctrl Pts',(5.24368657573216,-1.40331301745095,2.97635585162107));
#4986=CARTESIAN_POINT('Ctrl Pts',(5.2478343970707,-1.37832001504543,2.92408910459649));
#4987=CARTESIAN_POINT('Ctrl Pts',(5.25198221840925,-1.35043478546565,2.87328680009944));
#4988=CARTESIAN_POINT('Ctrl Pts',(5.2561300397478,-1.31986857258938,2.82427406330604));
#4989=CARTESIAN_POINT('Ctrl Pts',(5.25997653088088,-1.29152292864664,2.77882199531746));
#4990=CARTESIAN_POINT('Ctrl Pts',(5.26382302201397,-1.26087236047468,2.73490888339631));
#4991=CARTESIAN_POINT('Ctrl Pts',(5.26766951314705,-1.22811608950118,2.69276830024303));
#4992=CARTESIAN_POINT('Ctrl Pts',(5.27181796799075,-1.19278833069971,2.64731952621756));
#4993=CARTESIAN_POINT('Ctrl Pts',(5.27596642283445,-1.15486031021855,2.60373928251713));
#4994=CARTESIAN_POINT('Ctrl Pts',(5.28011487767815,-1.11455708914478,2.5623402092548));
#4995=CARTESIAN_POINT('Ctrl Pts',(5.28425596954489,-1.07432540113559,2.52101461405459));
#4996=CARTESIAN_POINT('Ctrl Pts',(5.28839706141163,-1.03172724032225,2.48186287528169));
#4997=CARTESIAN_POINT('Ctrl Pts',(5.29253815327836,-0.987028147397986,2.4451650033962));
#4998=CARTESIAN_POINT('Ctrl Pts',(5.29667513386998,-0.942373431723689,2.40850356515013));
#4999=CARTESIAN_POINT('Ctrl Pts',(5.30081211446159,-0.895622316970591,2.37429149565249));
#5000=CARTESIAN_POINT('Ctrl Pts',(5.3049490950532,-0.847076184934748,2.34277107936414));
#5001=CARTESIAN_POINT('Ctrl Pts',(5.3090835578996,-0.798559597826428,2.31126984623985));
#5002=CARTESIAN_POINT('Ctrl Pts',(5.31321802074599,-0.748250594795285,2.28245730203281));
#5003=CARTESIAN_POINT('Ctrl Pts',(5.31735248359239,-0.696480755874123,2.25653329379628));
#5004=CARTESIAN_POINT('Ctrl Pts',(5.32148601862379,-0.644722534624844,2.2306151031676));
#5005=CARTESIAN_POINT('Ctrl Pts',(5.32561955365519,-0.591504593667726,2.20758439462339));
#5006=CARTESIAN_POINT('Ctrl Pts',(5.32975308868659,-0.537182444298235,2.18759473149195));
#5007=CARTESIAN_POINT('Ctrl Pts',(5.3338903560124,-0.482811245809103,2.16758701908613));
#5008=CARTESIAN_POINT('Ctrl Pts',(5.33802762333821,-0.427334335914779,2.150626020662));
#5009=CARTESIAN_POINT('Ctrl Pts',(5.34216489066402,-0.371125235975002,2.1368163308734));
#5010=CARTESIAN_POINT('Ctrl Pts',(5.34630387138358,-0.314892857790565,2.12300092198703));
#5011=CARTESIAN_POINT('Ctrl Pts',(5.35044285210315,-0.257928197727282,2.11233952072552));
#5012=CARTESIAN_POINT('Ctrl Pts',(5.35458183282272,-0.20061472232637,2.10488547862257));
#5013=CARTESIAN_POINT('Ctrl Pts',(5.35872885786935,-0.143189855166912,2.09741694919614));
#5014=CARTESIAN_POINT('Ctrl Pts',(5.36287588291597,-0.0854153389819193,
2.09316827547533));
#5015=CARTESIAN_POINT('Ctrl Pts',(5.3670229079626,-0.0276785853040992,2.09214074431612));
#5016=CARTESIAN_POINT('Ctrl Pts',(5.37091428988111,0.0264989894077606,2.09117655525801));
#5017=CARTESIAN_POINT('Ctrl Pts',(5.37480567179962,0.0806429526473318,2.09304809442987));
#5018=CARTESIAN_POINT('Ctrl Pts',(5.37869705371814,0.134437993166185,2.0977149285101));
#5019=CARTESIAN_POINT('Ctrl Pts',(5.38284535886403,0.191784778467865,2.10268988399774));
#5020=CARTESIAN_POINT('Ctrl Pts',(5.38699366400992,0.248975180305846,2.11086278502762));
#5021=CARTESIAN_POINT('Ctrl Pts',(5.39114196915581,0.30562447496996,2.12221450175555));
#5022=CARTESIAN_POINT('Ctrl Pts',(5.39528291111001,0.362173217817999,2.13354606932294));
#5023=CARTESIAN_POINT('Ctrl Pts',(5.3994238530642,0.418182253502628,2.14804515179915));
#5024=CARTESIAN_POINT('Ctrl Pts',(5.4035647950184,0.473272264851125,2.16564090803079));
#5025=CARTESIAN_POINT('Ctrl Pts',(5.40770162566673,0.528307580459115,2.18321919443635));
#5026=CARTESIAN_POINT('Ctrl Pts',(5.41183845631507,0.58242518603099,2.20388790541525));
#5027=CARTESIAN_POINT('Ctrl Pts',(5.4159752869634,0.63525797006916,2.2275256146697));
#5028=CARTESIAN_POINT('Ctrl Pts',(5.42010960008704,0.6880586019962,2.25114893887388));
#5029=CARTESIAN_POINT('Ctrl Pts',(5.42424391321067,0.739575487986191,2.27773746746319));
#5030=CARTESIAN_POINT('Ctrl Pts',(5.42837822633431,0.789460743674109,2.30712136768179));
#5031=CARTESIAN_POINT('Ctrl Pts',(5.43251161211457,0.839334809894721,2.33649867697113));
#5032=CARTESIAN_POINT('Ctrl Pts',(5.43664499789482,0.887577523941647,2.36866984892292));
#5033=CARTESIAN_POINT('Ctrl Pts',(5.44077838367508,0.933866862659701,2.40341981708469));
#5034=CARTESIAN_POINT('Ctrl Pts',(5.44491550368043,0.980198020559258,2.43820117941337));
#5035=CARTESIAN_POINT('Ctrl Pts',(5.44905262368578,1.02457185839104,2.47556568122312));
#5036=CARTESIAN_POINT('Ctrl Pts',(5.45318974369113,1.06669768505829,2.51525653556928));
#5037=CARTESIAN_POINT('Ctrl Pts',(5.45732857790152,1.10884096645357,2.55496383571892));
#5038=CARTESIAN_POINT('Ctrl Pts',(5.46146741211191,1.14873401962117,2.59699903237818));
#5039=CARTESIAN_POINT('Ctrl Pts',(5.46560624632231,1.18612377654655,2.6410691547242));
#5040=CARTESIAN_POINT('Ctrl Pts',(5.4697531281496,1.22358623472658,2.68522496773663));
#5041=CARTESIAN_POINT('Ctrl Pts',(5.4739000099769,1.25853535357738,2.73142319730464));
#5042=CARTESIAN_POINT('Ctrl Pts',(5.4780468918042,1.29075963708495,2.77933928036531));
#5043=CARTESIAN_POINT('Ctrl Pts',(5.48193945929921,1.3210077135326,2.82431683101126));
#5044=CARTESIAN_POINT('Ctrl Pts',(5.48583202679421,1.34885515567857,2.87080740986868));
#5045=CARTESIAN_POINT('Ctrl Pts',(5.48972459428922,1.3741645240919,2.91852403348268));
#5046=CARTESIAN_POINT('Ctrl Pts',(5.49387311339754,1.40113808296194,2.96937821265901));
#5047=CARTESIAN_POINT('Ctrl Pts',(5.49802163250585,1.42534134831132,3.02183823319594));
#5048=CARTESIAN_POINT('Ctrl Pts',(5.50217015161417,1.44658140734486,3.07557064758019));
#5049=CARTESIAN_POINT('Ctrl Pts',(5.50631130597707,1.46778375951884,3.12920767237063));
#5050=CARTESIAN_POINT('Ctrl Pts',(5.51045246033997,1.48603315695587,3.18411212726835));
#5051=CARTESIAN_POINT('Ctrl Pts',(5.51459361470287,1.50118304248143,3.23992701809158));
#5052=CARTESIAN_POINT('Ctrl Pts',(5.51873065667904,1.51631788336419,3.29568648175706));
#5053=CARTESIAN_POINT('Ctrl Pts',(5.52286769865521,1.52835917507792,3.35235409006662));
#5054=CARTESIAN_POINT('Ctrl Pts',(5.52700474063139,1.53720946298209,3.40955562175472));
#5055=CARTESIAN_POINT('Ctrl Pts',(5.53113926366132,1.54605436215693,3.46672232479381));
#5056=CARTESIAN_POINT('Ctrl Pts',(5.53527378669126,1.55171202954511,3.52442179328069));
#5057=CARTESIAN_POINT('Ctrl Pts',(5.5394083097212,1.5541360973046,3.58226965692266));
#5058=CARTESIAN_POINT('Ctrl Pts',(5.54354190364442,1.55655962032951,3.6401045210389));
#5059=CARTESIAN_POINT('Ctrl Pts',(5.54767549756765,1.55575096456502,3.69808719414855));
#5060=CARTESIAN_POINT('Ctrl Pts',(5.55180909149087,1.5517157883933,3.75583044963218));
#5061=CARTESIAN_POINT('Ctrl Pts',(5.55594641523553,1.54767697120437,3.81362580796774));
#5062=CARTESIAN_POINT('Ctrl Pts',(5.56008373898019,1.54040585086493,3.87118079622951));
#5063=CARTESIAN_POINT('Ctrl Pts',(5.56422106272485,1.52996013383855,3.92811183302058));
#5064=CARTESIAN_POINT('Ctrl Pts',(5.56836009860536,1.51951009409348,3.98506642940609));
#5065=CARTESIAN_POINT('Ctrl Pts',(5.57249913448588,1.50588296008869,4.04139605210127));
#5066=CARTESIAN_POINT('Ctrl Pts',(5.5766381703664,1.48918725521302,4.09672905287659));
#5067=CARTESIAN_POINT('Ctrl Pts',(5.58078524774395,1.47245911320341,4.15216955698711));
#5068=CARTESIAN_POINT('Ctrl Pts',(5.5849323251215,1.45265066422468,4.20660907835341));
#5069=CARTESIAN_POINT('Ctrl Pts',(5.58907940249905,1.4299195384331,4.25969371179743));
#5070=CARTESIAN_POINT('Ctrl Pts',(5.59297031328613,1.40859252316597,4.30949928668583));
#5071=CARTESIAN_POINT('Ctrl Pts',(5.59686122407321,1.38469337269004,4.35811207240157));
#5072=CARTESIAN_POINT('Ctrl Pts',(5.60075213486029,1.35838814834895,4.40526113757677));
#5073=CARTESIAN_POINT('Ctrl Pts',(5.60490076102295,1.33034059139177,4.45553313198486));
#5074=CARTESIAN_POINT('Ctrl Pts',(5.60904938718561,1.29943983349391,4.50435122582026));
#5075=CARTESIAN_POINT('Ctrl Pts',(5.61319801334826,1.26586108932031,4.55137231787135));
#5076=CARTESIAN_POINT('Ctrl Pts',(5.61733927881018,1.23234192223975,4.5983099827412));
#5077=CARTESIAN_POINT('Ctrl Pts',(5.6214805442721,1.19615449993237,4.64345655405967));
#5078=CARTESIAN_POINT('Ctrl Pts',(5.62562180973402,1.15751898488018,4.68649506478161));
#5079=CARTESIAN_POINT('Ctrl Pts',(5.62975896518301,1.11892181377581,4.72949086178775));
#5080=CARTESIAN_POINT('Ctrl Pts',(5.63389612063199,1.07788170981579,4.77038235794146));
#5081=CARTESIAN_POINT('Ctrl Pts',(5.63803327608097,1.03465996895198,4.80888445904931));
#5082=CARTESIAN_POINT('Ctrl Pts',(5.64216791473878,0.991464521539555,4.84736313784459));
#5083=CARTESIAN_POINT('Ctrl Pts',(5.6463025533966,0.946090456058802,4.88345495740182));
#5084=CARTESIAN_POINT('Ctrl Pts',(5.65043719205441,0.898835336805132,4.91691220636806));
#5085=CARTESIAN_POINT('Ctrl Pts',(5.65457090354483,0.851590814222553,4.95036195275112));
#5086=CARTESIAN_POINT('Ctrl Pts',(5.65870461503524,0.802466500010036,4.98117800074397));
#5087=CARTESIAN_POINT('Ctrl Pts',(5.66283832652566,0.751790614076111,5.0091547711959));
#5088=CARTESIAN_POINT('Ctrl Pts',(5.66697576989225,0.701068978425046,5.03715679881524));
#5089=CARTESIAN_POINT('Ctrl Pts',(5.67111321325884,0.648793428175627,5.06231417327505));
#5090=CARTESIAN_POINT('Ctrl Pts',(5.67525065662543,0.595317392221242,5.08446699690548));
#5091=CARTESIAN_POINT('Ctrl Pts',(5.67938981344787,0.541819210023769,5.10662899477271));
#5092=CARTESIAN_POINT('Ctrl Pts',(5.68352897027031,0.487120043009846,5.12578378759081));
#5093=CARTESIAN_POINT('Ctrl Pts',(5.68766812709275,0.431590901758435,5.14182062688768));
#5094=CARTESIAN_POINT('Ctrl Pts',(5.69181532602098,0.375953871087131,5.15788862469429));
#5095=CARTESIAN_POINT('Ctrl Pts',(5.69596252494921,0.319484152727989,5.17082644518598));
#5096=CARTESIAN_POINT('Ctrl Pts',(5.70010972387744,0.26256453222091,5.18057420869907));
#5097=CARTESIAN_POINT('Ctrl Pts',(5.70399970772875,0.209175146173399,5.18971740228792));
#5098=CARTESIAN_POINT('Ctrl Pts',(5.70788969158006,0.155390369769301,5.19605443380859));
#5099=CARTESIAN_POINT('Ctrl Pts',(5.71177967543137,0.101527643020569,5.19957757207758));
#5100=CARTESIAN_POINT('Ctrl Pts',(5.71592728595477,0.0440976842286693,5.20333404149196));
#5101=CARTESIAN_POINT('Ctrl Pts',(5.72007489647816,-0.0136615881029595,
5.20390677509005));
#5102=CARTESIAN_POINT('Ctrl Pts',(5.72422250700156,-0.0713670981046394,
5.20125642718116));
#5103=CARTESIAN_POINT('Ctrl Pts',(5.72836275413177,-0.128970161563501,5.19861078452452));
#5104=CARTESIAN_POINT('Ctrl Pts',(5.73250300126198,-0.186519136065158,5.1927534414133));
#5105=CARTESIAN_POINT('Ctrl Pts',(5.73664324839219,-0.243628457187391,5.18369698564446));
#5106=CARTESIAN_POINT('Ctrl Pts',(5.74077938455052,-0.300681072802417,5.17464952229416));
#5107=CARTESIAN_POINT('Ctrl Pts',(5.74491552070884,-0.357294388064169,5.16240932097463));
#5108=CARTESIAN_POINT('Ctrl Pts',(5.74905165686716,-0.413087244050113,5.14704081952908));
#5109=CARTESIAN_POINT('Ctrl Pts',(5.75318527698905,-0.468846160907,5.13168166683518));
#5110=CARTESIAN_POINT('Ctrl Pts',(5.75731889711093,-0.523785106630128,5.11319812425796));
#5111=CARTESIAN_POINT('Ctrl Pts',(5.76145251723282,-0.577534600719312,5.09170538874802));
#5112=CARTESIAN_POINT('Ctrl Pts',(5.7655852126536,-0.631272070913043,5.07021746121644));
#5113=CARTESIAN_POINT('Ctrl Pts',(5.76971790807439,-0.683820134277736,5.045721870491));
#5114=CARTESIAN_POINT('Ctrl Pts',(5.77385060349517,-0.734828029057465,5.01838243967951));
#5115=CARTESIAN_POINT('Ctrl Pts',(5.77798704277871,-0.785882132555135,4.99101824172064));
#5116=CARTESIAN_POINT('Ctrl Pts',(5.78212348206224,-0.835392818450879,4.960805301017));
#5117=CARTESIAN_POINT('Ctrl Pts',(5.78625992134577,-0.883033984203595,4.92795342153106));
#5118=CARTESIAN_POINT('Ctrl Pts',(5.79039807897013,-0.930694940833091,4.89508789486649));
#5119=CARTESIAN_POINT('Ctrl Pts',(5.79453623659449,-0.97648441580041,4.85958156294093));
#5120=CARTESIAN_POINT('Ctrl Pts',(5.79867439421885,-1.02010802560609,4.82168568688939));
#5121=CARTESIAN_POINT('Ctrl Pts',(5.80282061530434,-1.06381663876689,4.78371596833321));
#5122=CARTESIAN_POINT('Ctrl Pts',(5.80696683638983,-1.10535057742057,4.74334776458121));
#5123=CARTESIAN_POINT('Ctrl Pts',(5.81111305747532,-1.14445177490562,4.70086985238897));
#5124=CARTESIAN_POINT('Ctrl Pts',(5.8150111103177,-1.18121260623954,4.66093441649565));
#5125=CARTESIAN_POINT('Ctrl Pts',(5.81890916316007,-1.21582333906808,4.61913487527536));
#5126=CARTESIAN_POINT('Ctrl Pts',(5.82280721600245,-1.24810396751099,4.57573531963284));
#5127=CARTESIAN_POINT('Ctrl Pts',(5.82697531032831,-1.28262086856104,4.52932921665444));
#5128=CARTESIAN_POINT('Ctrl Pts',(5.83114340465418,-1.3146187716897,4.48089784141534));
#5129=CARTESIAN_POINT('Ctrl Pts',(5.83531149898004,-1.34385418886963,4.43074379588781));
#5130=CARTESIAN_POINT('Ctrl Pts',(5.83947293308479,-1.3730428906138,4.38066989178867));
#5131=CARTESIAN_POINT('Ctrl Pts',(5.84363436718954,-1.3994776017878,4.32887921504193));
#5132=CARTESIAN_POINT('Ctrl Pts',(5.84779580129429,-1.4229568142114,4.27570502437007));
#5133=CARTESIAN_POINT('Ctrl Pts',(5.85195179078339,-1.44640530758853,4.22260040419334));
#5134=CARTESIAN_POINT('Ctrl Pts',(5.85610778027248,-1.46690577030666,4.16811633035365));
#5135=CARTESIAN_POINT('Ctrl Pts',(5.86026376976158,-1.48430262546907,4.11261051059714));
#5136=CARTESIAN_POINT('Ctrl Pts',(5.86441651567438,-1.50168590311234,4.05714801081562));
#5137=CARTESIAN_POINT('Ctrl Pts',(5.86856926158719,-1.51597022498911,4.00066583607906));
#5138=CARTESIAN_POINT('Ctrl Pts',(5.8727220075,-1.52704887102889,3.94353969530837));
#5139=CARTESIAN_POINT('Ctrl Pts',(5.87687406419901,-1.53812567839231,3.88642303552336));
#5140=CARTESIAN_POINT('Ctrl Pts',(5.88102612089801,-1.54599775636006,3.82866312385761));
#5141=CARTESIAN_POINT('Ctrl Pts',(5.88517817759702,-1.55060925665613,3.77064698619864));
#5142=CARTESIAN_POINT('Ctrl Pts',(5.88813752693258,-1.55389607119803,3.72929639036649));
#5143=CARTESIAN_POINT('Ctrl Pts',(5.89109687626814,-1.55552757156221,3.68781588946899));
#5144=CARTESIAN_POINT('Ctrl Pts',(5.8940562256037,-1.55549964733864,3.64634702884923));
#5145=CARTESIAN_POINT('Ctrl Pts',(5.05594377443823,-1.5554999873946,3.64759249708933));
#5146=CARTESIAN_POINT('Ctrl Pts',(5.06007749260067,-1.55550729033478,3.59022850230279));
#5147=CARTESIAN_POINT('Ctrl Pts',(5.06421121076312,-1.55233707856484,3.53274024496005));
#5148=CARTESIAN_POINT('Ctrl Pts',(5.06834492892557,-1.54597416002809,3.47551036045114));
#5149=CARTESIAN_POINT('Ctrl Pts',(5.07247136321427,-1.53962245335762,3.41838131863085));
#5150=CARTESIAN_POINT('Ctrl Pts',(5.07659779750297,-1.53008926129689,3.36151026343839));
#5151=CARTESIAN_POINT('Ctrl Pts',(5.08072423179167,-1.51741138191812,3.30527906666425));
#5152=CARTESIAN_POINT('Ctrl Pts',(5.08484662303307,-1.50474592422411,3.24910296476677));
#5153=CARTESIAN_POINT('Ctrl Pts',(5.08896901427447,-1.48894199726885,3.19356598886568));
#5154=CARTESIAN_POINT('Ctrl Pts',(5.09309140551587,-1.47008786542628,3.13904230892346));
#5155=CARTESIAN_POINT('Ctrl Pts',(5.09721137132577,-1.45124482651565,3.08455070828753));
#5156=CARTESIAN_POINT('Ctrl Pts',(5.10133133713566,-1.42935531067887,3.03107171707736));
#5157=CARTESIAN_POINT('Ctrl Pts',(5.10545130294555,-1.40455747949944,2.97896456411876));
#5158=CARTESIAN_POINT('Ctrl Pts',(5.10957045738072,-1.37976453193662,2.92686767299941));
#5159=CARTESIAN_POINT('Ctrl Pts',(5.11368961181589,-1.35206463182605,2.87614255733836));
#5160=CARTESIAN_POINT('Ctrl Pts',(5.11780876625106,-1.32164322904374,2.82712656989771));
#5161=CARTESIAN_POINT('Ctrl Pts',(5.12193169705873,-1.29119393642367,2.77806564541236));
#5162=CARTESIAN_POINT('Ctrl Pts',(5.1260546278664,-1.25801843387567,2.73071742648835));
#5163=CARTESIAN_POINT('Ctrl Pts',(5.13017755867406,-1.22234637900808,2.68539156822284));
#5164=CARTESIAN_POINT('Ctrl Pts',(5.13430235332377,-1.18665819797236,2.64004521962074));
#5165=CARTESIAN_POINT('Ctrl Pts',(5.13842714797347,-1.14847156347865,2.59672344769724));
#5166=CARTESIAN_POINT('Ctrl Pts',(5.14255194262318,-1.10805533127382,2.55570145610706));
#5167=CARTESIAN_POINT('Ctrl Pts',(5.14668451858051,-1.06756285499803,2.51460207769811));
#5168=CARTESIAN_POINT('Ctrl Pts',(5.15081709453784,-1.02483276916801,2.47581149899195));
#5169=CARTESIAN_POINT('Ctrl Pts',(5.15494967049517,-0.98016873643688,2.43956604581993));
#5170=CARTESIAN_POINT('Ctrl Pts',(5.15818677156541,-0.945182812488239,2.41117450590248));
#5171=CARTESIAN_POINT('Ctrl Pts',(5.16142387263565,-0.90901099518197,2.38434383327531));
#5172=CARTESIAN_POINT('Ctrl Pts',(5.16466097370589,-0.87181086109517,2.35916852828868));
#5173=CARTESIAN_POINT('Ctrl Pts',(5.16880939807082,-0.824137977463928,2.32690575788553));
#5174=CARTESIAN_POINT('Ctrl Pts',(5.17295782243574,-0.774571930974871,2.29722530939671));
#5175=CARTESIAN_POINT('Ctrl Pts',(5.17710624680067,-0.723423584423073,2.27035468400003));
#5176=CARTESIAN_POINT('Ctrl Pts',(5.18124730790192,-0.672366023849053,2.24353175273551));
#5177=CARTESIAN_POINT('Ctrl Pts',(5.18538836900317,-0.619732194895642,2.2195089855796));
#5178=CARTESIAN_POINT('Ctrl Pts',(5.18952943010441,-0.565861335505651,2.19847031603167));
#5179=CARTESIAN_POINT('Ctrl Pts',(5.19366637977742,-0.51204396148264,2.17745253460347));
#5180=CARTESIAN_POINT('Ctrl Pts',(5.19780332945043,-0.456992472997546,2.15941316913124));
#5181=CARTESIAN_POINT('Ctrl Pts',(5.20194027912344,-0.401068493576879,2.14448917736898));
#5182=CARTESIAN_POINT('Ctrl Pts',(5.20607471095171,-0.345178550803598,2.12957426869863));
#5183=CARTESIAN_POINT('Ctrl Pts',(5.21020914277998,-0.28841767179534,2.11777110909837));
#5184=CARTESIAN_POINT('Ctrl Pts',(5.21434357460825,-0.231163040437644,2.10916694976276));
#5185=CARTESIAN_POINT('Ctrl Pts',(5.2184770785754,-0.173921258329485,2.1005647213974));
#5186=CARTESIAN_POINT('Ctrl Pts',(5.22261058254255,-0.116186458521795,2.09516014532916));
#5187=CARTESIAN_POINT('Ctrl Pts',(5.2267440865097,-0.0583442347286329,2.09298905132408));
#5188=CARTESIAN_POINT('Ctrl Pts',(5.23088132294986,-0.000449780542021196,
2.09081599686371));
#5189=CARTESIAN_POINT('Ctrl Pts',(5.23501855939001,0.0575517699355676,2.09188227998785));
#5190=CARTESIAN_POINT('Ctrl Pts',(5.23915579583016,0.115272874994651,2.09617159123155));
#5191=CARTESIAN_POINT('Ctrl Pts',(5.24329474571062,0.17301788530289,2.10046267889748));
#5192=CARTESIAN_POINT('Ctrl Pts',(5.24743369559108,0.230481701072782,2.1079793893101));
#5193=CARTESIAN_POINT('Ctrl Pts',(5.25157264547153,0.287283205458235,2.11865361062956));
#5194=CARTESIAN_POINT('Ctrl Pts',(5.25571964016397,0.344195114037021,2.12934857926561));
#5195=CARTESIAN_POINT('Ctrl Pts',(5.2598666348564,0.400441631038254,2.143213199152));
#5196=CARTESIAN_POINT('Ctrl Pts',(5.26401362954884,0.455654023892158,2.16012863444283));
#5197=CARTESIAN_POINT('Ctrl Pts',(5.26790525779155,0.507466510599637,2.17600243959517));
#5198=CARTESIAN_POINT('Ctrl Pts',(5.27179688603426,0.558368129507118,2.19456229161852));
#5199=CARTESIAN_POINT('Ctrl Pts',(5.27568851427696,0.608071567144026,2.21567200242989));
#5200=CARTESIAN_POINT('Ctrl Pts',(5.27983691690473,0.661054498308648,2.23817455774597));
#5201=CARTESIAN_POINT('Ctrl Pts',(5.28398531953249,0.712897604072687,2.26366927627787));
#5202=CARTESIAN_POINT('Ctrl Pts',(5.28813372216025,0.763241019271921,2.2920187283133));
#5203=CARTESIAN_POINT('Ctrl Pts',(5.29227476151772,0.813495076661168,2.32031786105796));
#5204=CARTESIAN_POINT('Ctrl Pts',(5.29641580087518,0.862254277030835,2.35146141648703));
#5205=CARTESIAN_POINT('Ctrl Pts',(5.30055684023265,0.909179922442309,2.38526447552251));
#5206=CARTESIAN_POINT('Ctrl Pts',(5.30469376817226,0.956058977874934,2.41903397329758));
#5207=CARTESIAN_POINT('Ctrl Pts',(5.30883069611188,1.00110766483917,2.4554574402608));
#5208=CARTESIAN_POINT('Ctrl Pts',(5.3129676240515,1.04401456758386,2.49430564574127));
#5209=CARTESIAN_POINT('Ctrl Pts',(5.31710203419302,1.08689535652629,2.53313020760517));
#5210=CARTESIAN_POINT('Ctrl Pts',(5.32123644433453,1.12763656001703,2.57437623387099));
#5211=CARTESIAN_POINT('Ctrl Pts',(5.32537085447605,1.1659600447182,2.6177744295702));
#5212=CARTESIAN_POINT('Ctrl Pts',(5.32950433683933,1.20427492947547,2.66116288653999));
#5213=CARTESIAN_POINT('Ctrl Pts',(5.3336378192026,1.24017282806972,2.70670216401733));
#5214=CARTESIAN_POINT('Ctrl Pts',(5.33777130156588,1.2734142134817,2.75408797502258));
#5215=CARTESIAN_POINT('Ctrl Pts',(5.34190851670423,1.30668561779882,2.80151657817226));
#5216=CARTESIAN_POINT('Ctrl Pts',(5.34604573184259,1.33729541416731,2.85079462055169));
#5217=CARTESIAN_POINT('Ctrl Pts',(5.35018294698094,1.3650467945119,2.90158785877121));
#5218=CARTESIAN_POINT('Ctrl Pts',(5.35432187568943,1.39280966904645,2.9524021347597));
#5219=CARTESIAN_POINT('Ctrl Pts',(5.35846080439792,1.41771154198748,3.00473238704078));
#5220=CARTESIAN_POINT('Ctrl Pts',(5.36259973310641,1.43960258938017,3.05822162891506));
#5221=CARTESIAN_POINT('Ctrl Pts',(5.36674670712333,1.46153618890178,3.1118148439376));
#5222=CARTESIAN_POINT('Ctrl Pts',(5.37089368114024,1.48044709586661,3.16657105698239));
#5223=CARTESIAN_POINT('Ctrl Pts',(5.37504065515716,1.49623480202497,3.22211612741838));
#5224=CARTESIAN_POINT('Ctrl Pts',(5.37893245505412,1.51105104947425,3.27424336489753));
#5225=CARTESIAN_POINT('Ctrl Pts',(5.38282425495108,1.52311703828431,3.32706488305068));
#5226=CARTESIAN_POINT('Ctrl Pts',(5.38671605484805,1.53239104897987,3.3802654301649));
#5227=CARTESIAN_POINT('Ctrl Pts',(5.39086448300385,1.54227659502676,3.43697406200514));
#5228=CARTESIAN_POINT('Ctrl Pts',(5.39501291115965,1.54903070265895,3.49435094749466));
#5229=CARTESIAN_POINT('Ctrl Pts',(5.39916133931546,1.55257329113124,3.55201928458327));
#5230=CARTESIAN_POINT('Ctrl Pts',(5.40330240395167,1.55610959145807,3.60958525954483));
#5231=CARTESIAN_POINT('Ctrl Pts',(5.40744346858788,1.55644565569209,3.6674411438386));
#5232=CARTESIAN_POINT('Ctrl Pts',(5.41158453322409,1.55355277362111,3.7252021129864));
#5233=CARTESIAN_POINT('Ctrl Pts',(5.41572148627486,1.55066276383851,3.78290573235077));
#5234=CARTESIAN_POINT('Ctrl Pts',(5.41985843932563,1.54455018566779,3.84051410586875));
#5235=CARTESIAN_POINT('Ctrl Pts',(5.42399539237639,1.53523835277221,3.89764124683911));
#5236=CARTESIAN_POINT('Ctrl Pts',(5.42812982742146,1.52593218763452,3.95473361669534));
#5237=CARTESIAN_POINT('Ctrl Pts',(5.43226426246652,1.51343071143482,4.01134482177348));
#5238=CARTESIAN_POINT('Ctrl Pts',(5.43639869751159,1.49780895477388,4.06709505798939));
#5239=CARTESIAN_POINT('Ctrl Pts',(5.44053220453062,1.48219070461306,4.12283278036237));
#5240=CARTESIAN_POINT('Ctrl Pts',(5.44466571154965,1.46345370489618,4.17770941640907));
#5241=CARTESIAN_POINT('Ctrl Pts',(5.44879921856868,1.44172333621154,4.23135856976878));
#5242=CARTESIAN_POINT('Ctrl Pts',(5.45293645778093,1.41997334691554,4.28505616359459));
#5243=CARTESIAN_POINT('Ctrl Pts',(5.45707369699318,1.39522478243109,4.33752357571333));
#5244=CARTESIAN_POINT('Ctrl Pts',(5.46121093620544,1.36765137923423,4.38841400573123));
#5245=CARTESIAN_POINT('Ctrl Pts',(5.46534988870973,1.34006655748271,4.43932551022996));
#5246=CARTESIAN_POINT('Ctrl Pts',(5.46948884121402,1.30965483767951,4.48865828586473));
#5247=CARTESIAN_POINT('Ctrl Pts',(5.4736277937183,1.27663457277861,4.53609262715806));
#5248=CARTESIAN_POINT('Ctrl Pts',(5.47777479075219,1.24355012920017,4.583619162542));
#5249=CARTESIAN_POINT('Ctrl Pts',(5.48192178778607,1.20784733002492,4.62923947777156));
#5250=CARTESIAN_POINT('Ctrl Pts',(5.48606878481995,1.16978571820354,4.67266595598215));
#5251=CARTESIAN_POINT('Ctrl Pts',(5.48996038835301,1.13406813706523,4.71341800732238));
#5252=CARTESIAN_POINT('Ctrl Pts',(5.49385199188607,1.09627396077849,4.7522381990619));
#5253=CARTESIAN_POINT('Ctrl Pts',(5.49774359541912,1.05664517948853,4.78892029570244));
#5254=CARTESIAN_POINT('Ctrl Pts',(5.50189205063471,1.01440083906867,4.82802346585695));
#5255=CARTESIAN_POINT('Ctrl Pts',(5.50604050585029,0.969894475223361,4.86486035709219));
#5256=CARTESIAN_POINT('Ctrl Pts',(5.51018896106588,0.923398966675619,4.89915906210429));
#5257=CARTESIAN_POINT('Ctrl Pts',(5.51433005330703,0.876985981675375,4.93339689132644));
#5258=CARTESIAN_POINT('Ctrl Pts',(5.51847114554817,0.828591275070482,4.96510516952081));
#5259=CARTESIAN_POINT('Ctrl Pts',(5.52261223778932,0.778522364130185,4.99405076390987));
#5260=CARTESIAN_POINT('Ctrl Pts',(5.52674921875662,0.728503161574032,5.02296762113054));
#5261=CARTESIAN_POINT('Ctrl Pts',(5.53088619972392,0.676813496421476,5.04912696958262));
#5262=CARTESIAN_POINT('Ctrl Pts',(5.53502318069122,0.623790119403851,5.07233872576699));
#5263=CARTESIAN_POINT('Ctrl Pts',(5.53915764391395,0.570799012131047,5.09553635540019));
#5264=CARTESIAN_POINT('Ctrl Pts',(5.54329210713667,0.516476278018534,5.11578974041628));
#5265=CARTESIAN_POINT('Ctrl Pts',(5.54742657035939,0.461181567724821,5.1329555782995));
#5266=CARTESIAN_POINT('Ctrl Pts',(5.55156010576712,0.405899266118407,5.15011756399662));
#5267=CARTESIAN_POINT('Ctrl Pts',(5.55569364117484,0.349645918398539,5.16419322383587));
#5268=CARTESIAN_POINT('Ctrl Pts',(5.55982717658257,0.292797266398232,5.17508881297122));
#5269=CARTESIAN_POINT('Ctrl Pts',(5.5639644442817,0.23589728406829,5.18599424005633));
#5270=CARTESIAN_POINT('Ctrl Pts',(5.56810171198083,0.178401435691303,5.19371375896983));
#5271=CARTESIAN_POINT('Ctrl Pts',(5.57223897967996,0.120695275443563,5.19820486948887));
#5272=CARTESIAN_POINT('Ctrl Pts',(5.57637796077182,0.0629652169802013,5.2026978399398));
#5273=CARTESIAN_POINT('Ctrl Pts',(5.58051694186368,0.00502519466772049,
5.2039597239652));
#5274=CARTESIAN_POINT('Ctrl Pts',(5.58465592295554,-0.052737752275355,5.2020001994855));
#5275=CARTESIAN_POINT('Ctrl Pts',(5.58880294836785,-0.110612964446214,5.20003686657022));
#5276=CARTESIAN_POINT('Ctrl Pts',(5.59294997378016,-0.168309892939789,5.19483965925702));
#5277=CARTESIAN_POINT('Ctrl Pts',(5.59709699919246,-0.225446067434026,5.18647026910673));
#5278=CARTESIAN_POINT('Ctrl Pts',(5.60098837812504,-0.279060039765914,5.17861681626492));
#5279=CARTESIAN_POINT('Ctrl Pts',(5.60487975705762,-0.332179991546574,5.16797080129299));
#5280=CARTESIAN_POINT('Ctrl Pts',(5.6087711359902,-0.384501375266137,5.15462336344825));
#5281=CARTESIAN_POINT('Ctrl Pts',(5.61291944031003,-0.440277239262854,5.14039467099006));
#5282=CARTESIAN_POINT('Ctrl Pts',(5.61706774462986,-0.495379075984277,5.12303596400892));
#5283=CARTESIAN_POINT('Ctrl Pts',(5.62121604894968,-0.549430385441002,5.1026286424133));
#5284=CARTESIAN_POINT('Ctrl Pts',(5.62535699007877,-0.603385754467424,5.08225754357037));
#5285=CARTESIAN_POINT('Ctrl Pts',(5.62949793120785,-0.656293814205497,5.05884875313523));
#5286=CARTESIAN_POINT('Ctrl Pts',(5.63363887233693,-0.707791803328169,5.03253381619853));
#5287=CARTESIAN_POINT('Ctrl Pts',(5.63777570216127,-0.759238663028705,5.00624500586488));
#5288=CARTESIAN_POINT('Ctrl Pts',(5.64191253198561,-0.809277764543035,4.97705600153309));
#5289=CARTESIAN_POINT('Ctrl Pts',(5.64604936180995,-0.857566610935389,4.9451462773016));
#5290=CARTESIAN_POINT('Ctrl Pts',(5.65018367411206,-0.905826070514834,4.9132559721527));
#5291=CARTESIAN_POINT('Ctrl Pts',(5.65431798641418,-0.952336952841748,4.87864851574978));
#5292=CARTESIAN_POINT('Ctrl Pts',(5.65845229871629,-0.996783599410652,4.84154802036415));
#5293=CARTESIAN_POINT('Ctrl Pts',(5.66258568367884,-1.04122027645361,4.8044558467391));
#5294=CARTESIAN_POINT('Ctrl Pts',(5.66671906864139,-1.0835932373993,4.76487207783195));
#5295=CARTESIAN_POINT('Ctrl Pts',(5.67085245360394,-1.12361969242601,4.72306125534782));
#5296=CARTESIAN_POINT('Ctrl Pts',(5.67498957280401,-1.16368230868409,4.68121265957538));
#5297=CARTESIAN_POINT('Ctrl Pts',(5.67912669200407,-1.20139382085462,4.63713336577384));
#5298=CARTESIAN_POINT('Ctrl Pts',(5.68326381120414,-1.23650913495909,4.5911239894724));
#5299=CARTESIAN_POINT('Ctrl Pts',(5.68740264461471,-1.27163899905286,4.54509554923974));
#5300=CARTESIAN_POINT('Ctrl Pts',(5.69154147802527,-1.30417022656221,4.49713586336789));
#5301=CARTESIAN_POINT('Ctrl Pts',(5.69568031143583,-1.33390072694455,4.44757513579391));
#5302=CARTESIAN_POINT('Ctrl Pts',(5.69982719248294,-1.36368903595013,4.39791804127718));
#5303=CARTESIAN_POINT('Ctrl Pts',(5.70397407353005,-1.39066549083395,4.34665414594301));
#5304=CARTESIAN_POINT('Ctrl Pts',(5.70812095457716,-1.41467415468538,4.2941380697715));
#5305=CARTESIAN_POINT('Ctrl Pts',(5.71201352857186,-1.43721048970298,4.2448425365534));
#5306=CARTESIAN_POINT('Ctrl Pts',(5.71590610256657,-1.45713220257551,4.19444423214096));
#5307=CARTESIAN_POINT('Ctrl Pts',(5.71979867656128,-1.47435032060801,4.14324866270301));
#5308=CARTESIAN_POINT('Ctrl Pts',(5.7247075388849,-1.49606381173456,4.07868675526277));
#5309=CARTESIAN_POINT('Ctrl Pts',(5.72961640120853,-1.51355274598842,4.01263698113696));
#5310=CARTESIAN_POINT('Ctrl Pts',(5.73452526353215,-1.52664550808754,3.94561207781779));
#5311=CARTESIAN_POINT('Ctrl Pts',(5.73937986058867,-1.53959353558512,3.879328104686));
#5312=CARTESIAN_POINT('Ctrl Pts',(5.7442344576452,-1.54824196854562,3.81209054589745));
#5313=CARTESIAN_POINT('Ctrl Pts',(5.74908905470172,-1.55247128364616,3.74441592701353));
#5314=CARTESIAN_POINT('Ctrl Pts',(5.75137396126658,-1.55446188960699,3.71256360659188));
#5315=CARTESIAN_POINT('Ctrl Pts',(5.75365886783144,-1.55547421228667,3.68061475333113));
#5316=CARTESIAN_POINT('Ctrl Pts',(5.7559437743963,-1.5554995134887,3.64862472695888));
#5317=CARTESIAN_POINT('Origin',(1.2059437743963,0.,3.64739446828387));
#5318=CARTESIAN_POINT('',(6.5940562256037,-1.55549999978822,3.64736879997355));
#5319=CARTESIAN_POINT('',(6.4559437743963,-1.55498804050902,3.64654572419703));
#5320=CARTESIAN_POINT('',(1.2059437743963,-1.5555,3.64739446828386));
#5321=CARTESIAN_POINT('Ctrl Pts',(5.89405622564623,-1.55549964733824,3.64634702825331));
#5322=CARTESIAN_POINT('Ctrl Pts',(5.89876645506611,-1.55545520190131,3.58034338179285));
#5323=CARTESIAN_POINT('Ctrl Pts',(5.90347668448599,-1.55120566093629,3.51450400917026));
#5324=CARTESIAN_POINT('Ctrl Pts',(5.90818691390588,-1.54283758956267,3.44932270797349));
#5325=CARTESIAN_POINT('Ctrl Pts',(5.91293853705445,-1.53439597916469,3.38356859028381));
#5326=CARTESIAN_POINT('Ctrl Pts',(5.91769016020302,-1.52176325341198,3.31848438005927));
#5327=CARTESIAN_POINT('Ctrl Pts',(5.92244178335159,-1.50507796139423,3.25455788632466));
#5328=CARTESIAN_POINT('Ctrl Pts',(5.92623944109224,-1.49174251234766,3.20346567295395));
#5329=CARTESIAN_POINT('Ctrl Pts',(5.93003709883289,-1.47581937761418,3.1531126421748));
#5330=CARTESIAN_POINT('Ctrl Pts',(5.93383475657354,-1.45740100965981,3.10373782384496));
#5331=CARTESIAN_POINT('Ctrl Pts',(5.93798424644059,-1.43727628109979,3.04978869984821));
#5332=CARTESIAN_POINT('Ctrl Pts',(5.94213373630765,-1.4141099876031,2.99684609065118));
#5333=CARTESIAN_POINT('Ctrl Pts',(5.94628322617471,-1.38802361564245,2.94527575152803));
#5334=CARTESIAN_POINT('Ctrl Pts',(5.95042537286349,-1.36198340764075,2.89379667427226));
#5335=CARTESIAN_POINT('Ctrl Pts',(5.95456751955227,-1.33303361120314,2.84368550740766));
#5336=CARTESIAN_POINT('Ctrl Pts',(5.95870966624105,-1.30134408932065,2.79528895181879));
#5337=CARTESIAN_POINT('Ctrl Pts',(5.96284771292947,-1.26968593451924,2.7469403003507));
#5338=CARTESIAN_POINT('Ctrl Pts',(5.9669857596179,-1.23529371105071,2.70030333063743));
#5339=CARTESIAN_POINT('Ctrl Pts',(5.97112380630632,-1.19838275428231,2.65569944246255));
#5340=CARTESIAN_POINT('Ctrl Pts',(5.97525934459577,-1.16149417217827,2.61112259224915));
#5341=CARTESIAN_POINT('Ctrl Pts',(5.97939488288523,-1.1220902145225,2.56857678059709));
#5342=CARTESIAN_POINT('Ctrl Pts',(5.98353042117469,-1.08042771304446,2.5283519280355));
#5343=CARTESIAN_POINT('Ctrl Pts',(5.98766503908136,-1.03877448374493,2.48813602769715));
#5344=CARTESIAN_POINT('Ctrl Pts',(5.99179965698802,-0.994864082749133,2.45024042219371));
#5345=CARTESIAN_POINT('Ctrl Pts',(5.99593427489469,-0.948990009129827,2.41491801310439));
#5346=CARTESIAN_POINT('Ctrl Pts',(6.00007262786637,-0.903074494523489,2.379563695022));
#5347=CARTESIAN_POINT('Ctrl Pts',(6.00421098083804,-0.855192174986954,2.3467875377524));
#5348=CARTESIAN_POINT('Ctrl Pts',(6.00834933380971,-0.805668371193064,2.31680109476245));
#5349=CARTESIAN_POINT('Ctrl Pts',(6.01248940347486,-0.756124023672935,2.28680221263761));
#5350=CARTESIAN_POINT('Ctrl Pts',(6.01662947314,-0.704937294292704,2.25959559774776));
#5351=CARTESIAN_POINT('Ctrl Pts',(6.02076954280515,-0.652458312882652,2.2353468770355));
#5352=CARTESIAN_POINT('Ctrl Pts',(6.02491764792839,-0.599877475057004,2.21105109199942));
#5353=CARTESIAN_POINT('Ctrl Pts',(6.02906575305164,-0.545999858230309,2.18972486694799));
#5354=CARTESIAN_POINT('Ctrl Pts',(6.03321385817488,-0.491194922589014,2.17148532540861));
#5355=CARTESIAN_POINT('Ctrl Pts',(6.03709667116479,-0.439895037533872,2.15441229405697));
#5356=CARTESIAN_POINT('Ctrl Pts',(6.0409794841547,-0.387783153444902,2.14004335041998));
#5357=CARTESIAN_POINT('Ctrl Pts',(6.04486229714461,-0.335170067944933,2.12843387776357));
#5358=CARTESIAN_POINT('Ctrl Pts',(6.04900508487511,-0.279034259797718,2.11604708988489));
#5359=CARTESIAN_POINT('Ctrl Pts',(6.05314787260561,-0.222091363974047,2.10675003836955));
#5360=CARTESIAN_POINT('Ctrl Pts',(6.05729066033611,-0.164713239438949,2.10063986630154));
#5361=CARTESIAN_POINT('Ctrl Pts',(6.06142607839208,-0.107437185811405,2.09454056372104));
#5362=CARTESIAN_POINT('Ctrl Pts',(6.06556149644804,-0.0497279550305901,
2.09161694391283));
#5363=CARTESIAN_POINT('Ctrl Pts',(6.069696914504,0.00803220328821814,2.09191520654158));
#5364=CARTESIAN_POINT('Ctrl Pts',(6.07382822078269,0.0657349316439135,2.09221317261277));
#5365=CARTESIAN_POINT('Ctrl Pts',(6.07795952706138,0.123487967648581,2.09572667211674));
#5366=CARTESIAN_POINT('Ctrl Pts',(6.08209083334006,0.180905515728952,2.10244998889995));
#5367=CARTESIAN_POINT('Ctrl Pts',(6.08621963067589,0.23828819412462,2.10916922261197));
#5368=CARTESIAN_POINT('Ctrl Pts',(6.09034842801171,0.295335270781277,2.11909434928144));
#5369=CARTESIAN_POINT('Ctrl Pts',(6.09447722534754,0.351664776387409,2.13216770801055));
#5370=CARTESIAN_POINT('Ctrl Pts',(6.09860511296698,0.407981870661623,2.14523818622805));
#5371=CARTESIAN_POINT('Ctrl Pts',(6.10273300058642,0.463581199258392,2.16145540146296));
#5372=CARTESIAN_POINT('Ctrl Pts',(6.10686088820587,0.518091919598055,2.18071078976038));
#5373=CARTESIAN_POINT('Ctrl Pts',(6.11099258125585,0.57265289245891,2.19998392927815));
#5374=CARTESIAN_POINT('Ctrl Pts',(6.11512427430583,0.626122757588663,2.22230066550838));
#5375=CARTESIAN_POINT('Ctrl Pts',(6.11925596735582,0.678148079973918,2.24750324692855));
#5376=CARTESIAN_POINT('Ctrl Pts',(6.12338940431176,0.73019536121932,2.27271646586013));
#5377=CARTESIAN_POINT('Ctrl Pts',(6.12752284126771,0.780796426362209,2.30081770465715));
#5378=CARTESIAN_POINT('Ctrl Pts',(6.13165627822366,0.829622938255546,2.33160343992099));
#5379=CARTESIAN_POINT('Ctrl Pts',(6.13579788374345,0.878545941878112,2.36245001444441));
#5380=CARTESIAN_POINT('Ctrl Pts',(6.13993948926323,0.925686956785624,2.39599138361087));
#5381=CARTESIAN_POINT('Ctrl Pts',(6.14408109478302,0.970747883840817,2.43198145370052));
#5382=CARTESIAN_POINT('Ctrl Pts',(6.14801734242724,1.0135745043676,2.466186987745));
#5383=CARTESIAN_POINT('Ctrl Pts',(6.15195359007147,1.05452218822353,2.50260381659366));
#5384=CARTESIAN_POINT('Ctrl Pts',(6.15588983771569,1.09336663524267,2.54099054071577));
#5385=CARTESIAN_POINT('Ctrl Pts',(6.16004611115688,1.13438238376155,2.58152298084242));
#5386=CARTESIAN_POINT('Ctrl Pts',(6.16420238459808,1.1732257260731,2.62442275623431));
#5387=CARTESIAN_POINT('Ctrl Pts',(6.16835865803927,1.2096124064122,2.66942817221141));
#5388=CARTESIAN_POINT('Ctrl Pts',(6.17250750719807,1.24593408982704,2.71435319575958));
#5389=CARTESIAN_POINT('Ctrl Pts',(6.17665635635688,1.2798074992649,2.76137599322712));
#5390=CARTESIAN_POINT('Ctrl Pts',(6.18080520551568,1.31098563418944,2.81019860293998));
#5391=CARTESIAN_POINT('Ctrl Pts',(6.18494990073539,1.34213255272877,2.85897233014605));
#5392=CARTESIAN_POINT('Ctrl Pts',(6.1890945959551,1.37058926659055,2.90954186382701));
#5393=CARTESIAN_POINT('Ctrl Pts',(6.19323929117481,1.3961505096662,2.9615781631709));
#5394=CARTESIAN_POINT('Ctrl Pts',(6.19738141319725,1.42169588327081,3.01358215623988));
#5395=CARTESIAN_POINT('Ctrl Pts',(6.20152353521969,1.44434912188287,3.0670506450801));
#5396=CARTESIAN_POINT('Ctrl Pts',(6.20566565724214,1.46395068420032,3.1216296499198));
#5397=CARTESIAN_POINT('Ctrl Pts',(6.20980678316089,1.48354753270481,3.17619552951893));
#5398=CARTESIAN_POINT('Ctrl Pts',(6.21394790907965,1.50009398675634,3.23187090709963));
#5399=CARTESIAN_POINT('Ctrl Pts',(6.2180890349984,1.513479294399,3.28828351686983));
#5400=CARTESIAN_POINT('Ctrl Pts',(6.22223372590763,1.52687612511417,3.34474469082774));
#5401=CARTESIAN_POINT('Ctrl Pts',(6.22637841681686,1.53710624944037,3.40194385993305));
#5402=CARTESIAN_POINT('Ctrl Pts',(6.23052310772609,1.5441096675528,3.45949666475761));
#5403=CARTESIAN_POINT('Ctrl Pts',(6.23466943240518,1.55111584629894,3.51707215596342));
#5404=CARTESIAN_POINT('Ctrl Pts',(6.23881575708427,1.55489274683005,3.575001042381));
#5405=CARTESIAN_POINT('Ctrl Pts',(6.24296208176337,1.55543242157753,3.63289509224646));
#5406=CARTESIAN_POINT('Ctrl Pts',(6.24711622102969,1.55597311345118,3.69089825515485));
#5407=CARTESIAN_POINT('Ctrl Pts',(6.25127036029601,1.55326440933669,3.74886593033461));
#5408=CARTESIAN_POINT('Ctrl Pts',(6.25542449956233,1.54735052601686,3.80641207622514));
#5409=CARTESIAN_POINT('Ctrl Pts',(6.25925545913714,1.54189672524708,3.85948130295521));
#5410=CARTESIAN_POINT('Ctrl Pts',(6.26308641871195,1.53371769744794,3.9121917842015));
#5411=CARTESIAN_POINT('Ctrl Pts',(6.26691737828676,1.52288640708489,3.96424970512882));
#5412=CARTESIAN_POINT('Ctrl Pts',(6.27107106646946,1.51114266458232,4.02069310181546));
#5413=CARTESIAN_POINT('Ctrl Pts',(6.27522475465216,1.49623281783692,4.07659759798716));
#5414=CARTESIAN_POINT('Ctrl Pts',(6.27937844283485,1.47822260570092,4.13158263211564));
#5415=CARTESIAN_POINT('Ctrl Pts',(6.28352491304002,1.460243690403,4.18647211724689));
#5416=CARTESIAN_POINT('Ctrl Pts',(6.2876713832452,1.43917526453003,4.24044482260319));
#5417=CARTESIAN_POINT('Ctrl Pts',(6.29181785345036,1.41513374529266,4.29313182428395));
#5418=CARTESIAN_POINT('Ctrl Pts',(6.29596029630497,1.39111557691066,4.34576765255325));
#5419=CARTESIAN_POINT('Ctrl Pts',(6.30010273915958,1.3641302517053,4.39711978172299));
#5420=CARTESIAN_POINT('Ctrl Pts',(6.30424518201418,1.33434292531336,4.44683752921203));
#5421=CARTESIAN_POINT('Ctrl Pts',(6.30838518050274,1.30457317577931,4.49652593933218));
#5422=CARTESIAN_POINT('Ctrl Pts',(6.31252517899129,1.27200496925219,4.54458143538889));
#5423=CARTESIAN_POINT('Ctrl Pts',(6.31666517747985,1.23684919659391,4.59067826168064));
#5424=CARTESIAN_POINT('Ctrl Pts',(6.32080431108983,1.2017007682558,4.6367654579792));
#5425=CARTESIAN_POINT('Ctrl Pts',(6.32494344469982,1.16396616180008,4.68089438451619));
#5426=CARTESIAN_POINT('Ctrl Pts',(6.3290825783098,1.12389806613614,4.72277039647617));
#5427=CARTESIAN_POINT('Ctrl Pts',(6.33322549552921,1.08379334396076,4.76468468757585));
#5428=CARTESIAN_POINT('Ctrl Pts',(6.33736841274863,1.04135122909553,4.80434157222007));
#5429=CARTESIAN_POINT('Ctrl Pts',(6.34151132996804,0.996862078378707,4.84148250804077));
#5430=CARTESIAN_POINT('Ctrl Pts',(6.34565599776481,0.95235412890351,4.87863913765349));
#5431=CARTESIAN_POINT('Ctrl Pts',(6.34980066556158,0.905797835747466,4.91327738756307));
#5432=CARTESIAN_POINT('Ctrl Pts',(6.35394533335835,0.857514990188481,4.94518038730212));
#5433=CARTESIAN_POINT('Ctrl Pts',(6.35809803176834,0.809138592895799,4.97714520156145));
#5434=CARTESIAN_POINT('Ctrl Pts',(6.36225073017833,0.759029407425852,5.0063639114422));
#5435=CARTESIAN_POINT('Ctrl Pts',(6.36640342858832,0.707535639226755,5.03266468352131));
#5436=CARTESIAN_POINT('Ctrl Pts',(6.37025059201149,0.659830527519035,5.05703037501979));
#5437=CARTESIAN_POINT('Ctrl Pts',(6.37409775543467,0.610937638366414,5.07889208943651));
#5438=CARTESIAN_POINT('Ctrl Pts',(6.37794491885785,0.561147201320722,5.09815084633289));
#5439=CARTESIAN_POINT('Ctrl Pts',(6.38204949143226,0.50802534506297,5.11869818385905));
#5440=CARTESIAN_POINT('Ctrl Pts',(6.38615406400668,0.453648599692888,5.13637204992538));
#5441=CARTESIAN_POINT('Ctrl Pts',(6.3902586365811,0.398362951921499,5.15101915833667));
#5442=CARTESIAN_POINT('Ctrl Pts',(6.39437171253309,0.342962769754888,5.16569661092899));
#5443=CARTESIAN_POINT('Ctrl Pts',(6.39848478848509,0.286650394655892,5.17733450259257));
#5444=CARTESIAN_POINT('Ctrl Pts',(6.40259786443708,0.229794572184286,5.18582701623475));
#5445=CARTESIAN_POINT('Ctrl Pts',(6.40669109440536,0.173213084478161,5.19427855268872));
#5446=CARTESIAN_POINT('Ctrl Pts',(6.41078432437364,0.116093905813112,5.19961488454923));
#5447=CARTESIAN_POINT('Ctrl Pts',(6.41487755434192,0.058813295256594,5.20178220829634));
#5448=CARTESIAN_POINT('Ctrl Pts',(6.41896840146112,0.00156603026121408,
5.20394827034903));
#5449=CARTESIAN_POINT('Ctrl Pts',(6.42305924858032,-0.0558419493354018,
5.20294895786843));
#5450=CARTESIAN_POINT('Ctrl Pts',(6.42715009569952,-0.113030086156676,5.19878237903457));
#5451=CARTESIAN_POINT('Ctrl Pts',(6.43124021285904,-0.170208018481599,5.19461654367375));
#5452=CARTESIAN_POINT('Ctrl Pts',(6.43533033001855,-0.227165654833645,5.18728460211641));
#5453=CARTESIAN_POINT('Ctrl Pts',(6.43942044717806,-0.283525656181346,5.17683667127388));
#5454=CARTESIAN_POINT('Ctrl Pts',(6.4435497815323,-0.340426053087751,5.16628856272926));
#5455=CARTESIAN_POINT('Ctrl Pts',(6.44767911588654,-0.396716744592947,5.15256446132537));
#5456=CARTESIAN_POINT('Ctrl Pts',(6.45180845024078,-0.45202073919452,5.13576858164988));
#5457=CARTESIAN_POINT('Ctrl Pts',(6.45590494376929,-0.506884898051893,5.11910628053936));
#5458=CARTESIAN_POINT('Ctrl Pts',(6.4600014372978,-0.560777515795708,5.0994211367842));
#5459=CARTESIAN_POINT('Ctrl Pts',(6.46409793082631,-0.613349278357512,5.07686391977219));
#5460=CARTESIAN_POINT('Ctrl Pts',(6.46824368559341,-0.666553227964335,5.05403544724825));
#5461=CARTESIAN_POINT('Ctrl Pts',(6.47238944036051,-0.718403838885281,5.02826561058247));
#5462=CARTESIAN_POINT('Ctrl Pts',(6.47653519512761,-0.768565993296113,4.99975779370673));
#5463=CARTESIAN_POINT('Ctrl Pts',(6.48068094989472,-0.818728147706942,4.97124997683098));
#5464=CARTESIAN_POINT('Ctrl Pts',(6.48482670466182,-0.86720142445848,4.94000455072264));
#5465=CARTESIAN_POINT('Ctrl Pts',(6.48897245942892,-0.913684566917064,4.90626728242261));
#5466=CARTESIAN_POINT('Ctrl Pts',(6.4933509496862,-0.962777192462079,4.87063606232941));
#5467=CARTESIAN_POINT('Ctrl Pts',(6.49772943994349,-1.00987680836232,4.83206076559067));
#5468=CARTESIAN_POINT('Ctrl Pts',(6.50210793020077,-1.05462032230713,4.79079126108015));
#5469=CARTESIAN_POINT('Ctrl Pts',(6.50633096419065,-1.09777523852538,4.75098701120122));
#5470=CARTESIAN_POINT('Ctrl Pts',(6.51055399818052,-1.13873813199972,4.70867701401803));
#5471=CARTESIAN_POINT('Ctrl Pts',(6.5147770321704,-1.17721363608816,4.66412860512009));
#5472=CARTESIAN_POINT('Ctrl Pts',(6.51899490443744,-1.2156421124026,4.61963464677595));
#5473=CARTESIAN_POINT('Ctrl Pts',(6.52321277670448,-1.25158891032136,4.5729080796287));
#5474=CARTESIAN_POINT('Ctrl Pts',(6.52743064897153,-1.28479547448399,4.52425297382821));
#5475=CARTESIAN_POINT('Ctrl Pts',(6.53164476649455,-1.31797247820946,4.47564118073514));
#5476=CARTESIAN_POINT('Ctrl Pts',(6.53585888401758,-1.3484138122942,4.42510466592988));
#5477=CARTESIAN_POINT('Ctrl Pts',(6.5400730015406,-1.3759023907967,4.37297896439712));
#5478=CARTESIAN_POINT('Ctrl Pts',(6.5442847660271,-1.40337562050344,4.32088236828888));
#5479=CARTESIAN_POINT('Ctrl Pts',(6.5484965305136,-1.42789913910852,4.26719878661905));
#5480=CARTESIAN_POINT('Ctrl Pts',(6.55270829500011,-1.4493012164244,4.21228935591408));
#5481=CARTESIAN_POINT('Ctrl Pts',(6.55692040483961,-1.47070504865126,4.1573754227881));
#5482=CARTESIAN_POINT('Ctrl Pts',(6.56113251467912,-1.4889867388586,4.10123589863111));
#5483=CARTESIAN_POINT('Ctrl Pts',(6.56534462451863,-1.50402284555278,4.04425153330266));
#5484=CARTESIAN_POINT('Ctrl Pts',(6.56955693078515,-1.51905965343891,3.9872645105723));
#5485=CARTESIAN_POINT('Ctrl Pts',(6.57376923705167,-1.53085045935568,3.92943305061999));
#5486=CARTESIAN_POINT('Ctrl Pts',(6.5779815433182,-1.53932242567223,3.87115040635603));
#5487=CARTESIAN_POINT('Ctrl Pts',(6.58219714361556,-1.54780101708121,3.81282218496265));
#5488=CARTESIAN_POINT('Ctrl Pts',(6.58641274391292,-1.55295552961871,3.75404256799044));
#5489=CARTESIAN_POINT('Ctrl Pts',(6.59062834421029,-1.55476488354477,3.6952108556006));
#5490=CARTESIAN_POINT('Ctrl Pts',(6.59177097134143,-1.55525530406377,3.6792646780681));
#5491=CARTESIAN_POINT('Ctrl Pts',(6.59291359847256,-1.55550026292146,3.66331467869627));
#5492=CARTESIAN_POINT('Ctrl Pts',(6.5940562256037,-1.55549999978822,3.64736879997355));
#5493=CARTESIAN_POINT('Ctrl Pts',(5.7559437743963,-1.55415988380114,3.64862366743361));
#5494=CARTESIAN_POINT('Ctrl Pts',(5.78090458864165,-1.55156969786396,3.29945639063284));
#5495=CARTESIAN_POINT('Ctrl Pts',(5.84287458307737,-1.26257785748728,2.42869791902303));
#5496=CARTESIAN_POINT('Ctrl Pts',(5.94185375770342,0.17968266065122,1.81826775193874));
#5497=CARTESIAN_POINT('Ctrl Pts',(6.05288129827453,1.63338127522104,2.80478342088779));
#5498=CARTESIAN_POINT('Ctrl Pts',(6.16390883884558,1.5946610617751,4.56100604319437));
#5499=CARTESIAN_POINT('Ctrl Pts',(6.27493637941668,0.0991443931483699,5.48278383251785));
#5500=CARTESIAN_POINT('Ctrl Pts',(6.37228135793357,-1.29176384967164,4.82025828670267));
#5501=CARTESIAN_POINT('Ctrl Pts',(6.43261715626011,-1.55167090461383,3.97306868873034));
#5502=CARTESIAN_POINT('Ctrl Pts',(6.4559437743963,-1.55356356749417,3.64654650170336));
#5503=CARTESIAN_POINT('Origin',(0.,0.,3.64739446828387));
#5504=CARTESIAN_POINT('',(2.72586969217418,-1.95399957629683,3.64868125956087));
#5505=CARTESIAN_POINT('',(2.6241303079204,-1.95399895847038,3.64941196591101));
#5506=CARTESIAN_POINT('',(0.,-1.954,3.64739446828387));
#5507=CARTESIAN_POINT('',(2.50004110459941,0.86152797471893,5.40121474093917));
#5508=CARTESIAN_POINT('Ctrl Pts',(2.72586969212423,-1.95399957629626,3.64868126043292));
#5509=CARTESIAN_POINT('Ctrl Pts',(2.72192515475357,-1.95395422424648,3.71754854884412));
#5510=CARTESIAN_POINT('Ctrl Pts',(2.71798061738291,-1.95026833624108,3.78630291233304));
#5511=CARTESIAN_POINT('Ctrl Pts',(2.71403608001225,-1.94297611333583,3.85466198384382));
#5512=CARTESIAN_POINT('Ctrl Pts',(2.71011016029676,-1.93571830868518,3.92269841026298));
#5513=CARTESIAN_POINT('Ctrl Pts',(2.70618424058128,-1.92486848969711,3.99048552896683));
#5514=CARTESIAN_POINT('Ctrl Pts',(2.70225832086579,-1.91045410367946,4.05761528410667));
#5515=CARTESIAN_POINT('Ctrl Pts',(2.69833831584264,-1.89606143401484,4.12464390323834));
#5516=CARTESIAN_POINT('Ctrl Pts',(2.69441831081949,-1.87811495873734,4.19101664947758));
#5517=CARTESIAN_POINT('Ctrl Pts',(2.69049830579634,-1.85669380632836,4.25633133655668));
#5518=CARTESIAN_POINT('Ctrl Pts',(2.6865829619205,-1.83529812509765,4.32156836011862));
#5519=CARTESIAN_POINT('Ctrl Pts',(2.68266761804465,-1.81043612540169,4.38574936031743));
#5520=CARTESIAN_POINT('Ctrl Pts',(2.6787522741688,-1.78223740886531,4.44848486171089));
#5521=CARTESIAN_POINT('Ctrl Pts',(2.67483942124938,-1.75405663245792,4.5111804505436));
#5522=CARTESIAN_POINT('Ctrl Pts',(2.67092656832996,-1.7225435511983,4.57243191939858));
#5523=CARTESIAN_POINT('Ctrl Pts',(2.66701371541053,-1.68787623580068,4.63186885221639));
#5524=CARTESIAN_POINT('Ctrl Pts',(2.663102024005,-1.65321921124944,4.69128814143135));
#5525=CARTESIAN_POINT('Ctrl Pts',(2.65919033259946,-1.61541005819062,4.74889354119087));
#5526=CARTESIAN_POINT('Ctrl Pts',(2.65527864119393,-1.57467238540547,4.80433996338788));
#5527=CARTESIAN_POINT('Ctrl Pts',(2.65136678355455,-1.53393298140502,4.859788741873));
#5528=CARTESIAN_POINT('Ctrl Pts',(2.64745492591517,-1.49026510259596,4.91307796744342));
#5529=CARTESIAN_POINT('Ctrl Pts',(2.64354306827579,-1.44393413822889,4.96389369139689));
#5530=CARTESIAN_POINT('Ctrl Pts',(2.63962720909831,-1.39755578074682,5.01476139603935));
#5531=CARTESIAN_POINT('Ctrl Pts',(2.63571134992084,-1.34850923151089,5.06315018672228));
#5532=CARTESIAN_POINT('Ctrl Pts',(2.63179549074336,-1.29709774028617,5.10878197751765));
#5533=CARTESIAN_POINT('Ctrl Pts',(2.6278773663268,-1.24565650863569,5.15444016530821));
#5534=CARTESIAN_POINT('Ctrl Pts',(2.62395924191025,-1.19184799458207,5.19733787283971));
#5535=CARTESIAN_POINT('Ctrl Pts',(2.62004111749369,-1.13600746521167,5.23723818355382));
#5536=CARTESIAN_POINT('Ctrl Pts',(2.61611645127961,-1.08007370311117,5.27720511281438));
#5537=CARTESIAN_POINT('Ctrl Pts',(2.61219178506554,-1.0221015668269,5.31416439325073));
#5538=CARTESIAN_POINT('Ctrl Pts',(2.60826711885147,-0.962453365995261,5.34792365600291));
#5539=CARTESIAN_POINT('Ctrl Pts',(2.60651425904804,-0.935812900823969,5.36300143623801));
#5540=CARTESIAN_POINT('Ctrl Pts',(2.6047613992446,-0.908838399945064,5.37744152154705));
#5541=CARTESIAN_POINT('Ctrl Pts',(2.60300853944117,-0.881563413985287,5.39122988113756));
#5542=CARTESIAN_POINT('Ctrl Pts',(2.59912724522269,-0.821169396672931,5.42176094828629));
#5543=CARTESIAN_POINT('Ctrl Pts',(2.59524595100421,-0.759058631374259,5.44921582459445));
#5544=CARTESIAN_POINT('Ctrl Pts',(2.59136465678574,-0.695580341215257,5.47339665582771));
#5545=CARTESIAN_POINT('Ctrl Pts',(2.58748986314907,-0.632208367608115,5.49753698781955));
#5546=CARTESIAN_POINT('Ctrl Pts',(2.58361506951239,-0.567473881608454,5.51841398464901));
#5547=CARTESIAN_POINT('Ctrl Pts',(2.57974027587572,-0.50174941555497,5.53587627227094));
#5548=CARTESIAN_POINT('Ctrl Pts',(2.57586910437471,-0.436086388368726,5.55332223624301));
#5549=CARTESIAN_POINT('Ctrl Pts',(2.57199793287369,-0.369435697939428,5.56735968916254));
#5550=CARTESIAN_POINT('Ctrl Pts',(2.56812676137267,-0.302187103605631,5.57788636270209));
#5551=CARTESIAN_POINT('Ctrl Pts',(2.56425781933617,-0.23497723872495,5.58840697377574));
#5552=CARTESIAN_POINT('Ctrl Pts',(2.56038887729968,-0.16717064773718,5.5954207372019));
#5553=CARTESIAN_POINT('Ctrl Pts',(2.55651993526318,-0.0991674998868228,
5.59887641976746));
#5554=CARTESIAN_POINT('Ctrl Pts',(2.55265183306664,-0.0311791136327506,
5.60233135220023));
#5555=CARTESIAN_POINT('Ctrl Pts',(2.54878373087009,0.0370052435431303,5.60222971205842));
#5556=CARTESIAN_POINT('Ctrl Pts',(2.54491562867355,0.104982014579131,5.59857226044298));
#5557=CARTESIAN_POINT('Ctrl Pts',(2.54104440908414,0.173013569664301,5.59491186120284));
#5558=CARTESIAN_POINT('Ctrl Pts',(2.53717318949473,0.240836701823915,5.58768995036121));
#5559=CARTESIAN_POINT('Ctrl Pts',(2.53330196990532,0.308050758920962,5.57695937518082));
#5560=CARTESIAN_POINT('Ctrl Pts',(2.52942926989751,0.375290519785128,5.566224696451));
#5561=CARTESIAN_POINT('Ctrl Pts',(2.52555656988971,0.441920249618249,5.55197878458951));
#5562=CARTESIAN_POINT('Ctrl Pts',(2.5216838698819,0.507550177318446,5.53432552624651));
#5563=CARTESIAN_POINT('Ctrl Pts',(2.51780443308886,0.573294272066705,5.51664155904151));
#5564=CARTESIAN_POINT('Ctrl Pts',(2.51392499629581,0.638034611784042,5.49553856038448));
#5565=CARTESIAN_POINT('Ctrl Pts',(2.51004555950277,0.701398004787308,5.47116990371456));
#5566=CARTESIAN_POINT('Ctrl Pts',(2.50671074120165,0.755866066488274,5.4502222645154));
#5567=CARTESIAN_POINT('Ctrl Pts',(2.50337592290053,0.809316799860291,5.42686240189679));
#5568=CARTESIAN_POINT('Ctrl Pts',(2.50004110459941,0.86152797471893,5.40121474093917));
#5569=CARTESIAN_POINT('',(2.5,-0.861525859670532,5.40121577991141));
#5570=CARTESIAN_POINT('Origin',(2.5,0.,3.64739446828387));
#5571=CARTESIAN_POINT('Ctrl Pts',(2.5,-0.861525859670532,5.40121577991141));
#5572=CARTESIAN_POINT('Ctrl Pts',(2.50400926879465,-0.924640824599854,5.37021195183708));
#5573=CARTESIAN_POINT('Ctrl Pts',(2.5080185375893,-0.986127805684975,5.33577388677798));
#5574=CARTESIAN_POINT('Ctrl Pts',(2.51202780638395,-1.04560615745962,5.29809848884072));
#5575=CARTESIAN_POINT('Ctrl Pts',(2.51615279530842,-1.1068012418708,5.25933566021138));
#5576=CARTESIAN_POINT('Ctrl Pts',(2.52027778423288,-1.16586949339279,5.21714593155206));
#5577=CARTESIAN_POINT('Ctrl Pts',(2.52440277315734,-1.22242491847297,5.17179379874041));
#5578=CARTESIAN_POINT('Ctrl Pts',(2.52840911791387,-1.27735367946413,5.1277460975673));
#5579=CARTESIAN_POINT('Ctrl Pts',(2.53241546267039,-1.32991185917089,5.08071578688039));
#5580=CARTESIAN_POINT('Ctrl Pts',(2.53642180742692,-1.37977792362143,5.03098721236969));
#5581=CARTESIAN_POINT('Ctrl Pts',(2.54042822966511,-1.42964495246871,4.98125767612127));
#5582=CARTESIAN_POINT('Ctrl Pts',(2.5444346519033,-1.47681943741634,4.92883009647148));
#5583=CARTESIAN_POINT('Ctrl Pts',(2.54844107414149,-1.52101670404322,4.87402570301643));
#5584=CARTESIAN_POINT('Ctrl Pts',(2.55244865861312,-1.56522679197001,4.81920541121248));
#5585=CARTESIAN_POINT('Ctrl Pts',(2.55645624308475,-1.60645765682523,4.76200729257378));
#5586=CARTESIAN_POINT('Ctrl Pts',(2.56046382755638,-1.64446579811897,4.70278455674261));
#5587=CARTESIAN_POINT('Ctrl Pts',(2.56467747030761,-1.68442820694246,4.64051676093959));
#5588=CARTESIAN_POINT('Ctrl Pts',(2.56889111305883,-1.72082726588746,4.57601102517087));
#5589=CARTESIAN_POINT('Ctrl Pts',(2.57310475581006,-1.75343383018518,4.50970868199146));
#5590=CARTESIAN_POINT('Ctrl Pts',(2.57712095959757,-1.78451254633696,4.4465130725106));
#5591=CARTESIAN_POINT('Ctrl Pts',(2.58113716338509,-1.81214608686427,4.38168590917152));
#5592=CARTESIAN_POINT('Ctrl Pts',(2.5851533671726,-1.83618572392645,4.3156294473509));
#5593=CARTESIAN_POINT('Ctrl Pts',(2.58917326103715,-1.86024744854125,4.24951229303426));
#5594=CARTESIAN_POINT('Ctrl Pts',(2.59319315490169,-1.8807085593928,4.18216402918133));
#5595=CARTESIAN_POINT('Ctrl Pts',(2.59721304876624,-1.89747052412525,4.1140009513891));
#5596=CARTESIAN_POINT('Ctrl Pts',(2.6012402368791,-1.91426290407195,4.04571418913341));
#5597=CARTESIAN_POINT('Ctrl Pts',(2.60526742499197,-1.92734265511497,3.97661011190267));
#5598=CARTESIAN_POINT('Ctrl Pts',(2.60929461310484,-1.93666260885462,3.90711343074987));
#5599=CARTESIAN_POINT('Ctrl Pts',(2.60987225559358,-1.93799942281074,3.89714512662903));
#5600=CARTESIAN_POINT('Ctrl Pts',(2.61044989808233,-1.93925897094148,3.88716874862355));
#5601=CARTESIAN_POINT('Ctrl Pts',(2.61102754057108,-1.94044120187923,3.87718555176946));
#5602=CARTESIAN_POINT('Ctrl Pts',(2.61539512967265,-1.94938012008528,3.80170200852605));
#5603=CARTESIAN_POINT('Ctrl Pts',(2.61976271877421,-1.95392024650498,3.72564652348674));
#5604=CARTESIAN_POINT('Ctrl Pts',(2.62413030787577,-1.95399895846957,3.64941196669006));
#5605=CARTESIAN_POINT('Origin',(0.,0.,3.64739446828387));
#5606=CARTESIAN_POINT('',(3.42586969208078,-1.95399979033444,3.64829966051471));
#5607=CARTESIAN_POINT('',(3.3241303078362,-1.95399983251307,3.64820350405597));
#5608=CARTESIAN_POINT('',(0.,-1.954,3.64739446828387));
#5609=CARTESIAN_POINT('Ctrl Pts',(3.42586969208078,-1.95399979033444,3.64829966051471));
#5610=CARTESIAN_POINT('Ctrl Pts',(3.42158392528816,-1.95396480342059,3.72382441647484));
#5611=CARTESIAN_POINT('Ctrl Pts',(3.41729815849555,-1.94954693631289,3.79920428739692));
#5612=CARTESIAN_POINT('Ctrl Pts',(3.41301239170294,-1.94082130003993,3.87395280803618));
#5613=CARTESIAN_POINT('Ctrl Pts',(3.40871252448995,-1.93206695591947,3.94894725562724));
#5614=CARTESIAN_POINT('Ctrl Pts',(3.40441265727697,-1.91897658649658,4.0233058867645));
#5615=CARTESIAN_POINT('Ctrl Pts',(3.40011279006398,-1.90167612158761,4.09655360331678));
#5616=CARTESIAN_POINT('Ctrl Pts',(3.39579316317008,-1.88429615383603,4.1701379236373));
#5617=CARTESIAN_POINT('Ctrl Pts',(3.39147353627618,-1.86266745413098,4.24260079990365));
#5618=CARTESIAN_POINT('Ctrl Pts',(3.38715390938228,-1.83696603276114,4.3134813954051));
#5619=CARTESIAN_POINT('Ctrl Pts',(3.38483638073443,-1.82317692972559,4.35150963596525));
#5620=CARTESIAN_POINT('Ctrl Pts',(3.38251885208658,-1.80821632797972,4.3890828085135));
#5621=CARTESIAN_POINT('Ctrl Pts',(3.38020132343873,-1.79211686507899,4.4261326411632));
#5622=CARTESIAN_POINT('Ctrl Pts',(3.37628273639694,-1.76489513180678,4.48877825042292));
#5623=CARTESIAN_POINT('Ctrl Pts',(3.37236414935515,-1.73433083910883,4.55011866002973));
#5624=CARTESIAN_POINT('Ctrl Pts',(3.36844556231337,-1.70057119742648,4.60977360484257));
#5625=CARTESIAN_POINT('Ctrl Pts',(3.36453286752669,-1.66686231904712,4.669338848406));
#5626=CARTESIAN_POINT('Ctrl Pts',(3.36062017274002,-1.62996786774874,4.72722323253677));
#5627=CARTESIAN_POINT('Ctrl Pts',(3.35670747795334,-1.59008264753985,4.78306747315484));
#5628=CARTESIAN_POINT('Ctrl Pts',(3.35279937593377,-1.55024424507097,4.83884616314728));
#5629=CARTESIAN_POINT('Ctrl Pts',(3.3488912739142,-1.50742233031501,4.89258906739674));
#5630=CARTESIAN_POINT('Ctrl Pts',(3.34498317189463,-1.46185610518546,4.94396406831775));
#5631=CARTESIAN_POINT('Ctrl Pts',(3.34107751390498,-1.4163183760412,4.99530694058938));
#5632=CARTESIAN_POINT('Ctrl Pts',(3.33717185591533,-1.36804006657401,5.044284479995));
#5633=CARTESIAN_POINT('Ctrl Pts',(3.33326619792568,-1.3173009502997,5.0905972282381));
#5634=CARTESIAN_POINT('Ctrl Pts',(3.32936164377851,-1.26657617424465,5.13689688727089));
#5635=CARTESIAN_POINT('Ctrl Pts',(3.32545708963134,-1.21339233509802,5.18053291892595));
#5636=CARTESIAN_POINT('Ctrl Pts',(3.32155253548417,-1.15806508986369,5.22124365027019));
#5637=CARTESIAN_POINT('Ctrl Pts',(3.31764774663011,-1.10273451885,5.26195682877965));
#5638=CARTESIAN_POINT('Ctrl Pts',(3.31374295777605,-1.04526068354753,5.29974406850757));
#5639=CARTESIAN_POINT('Ctrl Pts',(3.30983816892199,-0.985989779129678,5.33438591919636));
#5640=CARTESIAN_POINT('Ctrl Pts',(3.30592922772634,-0.926655846197141,5.36906460793269));
#5641=CARTESIAN_POINT('Ctrl Pts',(3.30202028653069,-0.865521455784667,5.40059098391655));
#5642=CARTESIAN_POINT('Ctrl Pts',(3.29811134533503,-0.802958182434663,5.42879115551028));
#5643=CARTESIAN_POINT('Ctrl Pts',(3.29420006241485,-0.740357429382513,5.45700822094564));
#5644=CARTESIAN_POINT('Ctrl Pts',(3.29028877949467,-0.676326548180478,5.48189493811238));
#5645=CARTESIAN_POINT('Ctrl Pts',(3.2863774965745,-0.611255279002647,5.50332630536502));
#5646=CARTESIAN_POINT('Ctrl Pts',(3.28245948400635,-0.546072049952974,5.5247945468505));
#5647=CARTESIAN_POINT('Ctrl Pts',(3.2785414714382,-0.479845334551296,5.54279544405974));
#5648=CARTESIAN_POINT('Ctrl Pts',(3.27462345887005,-0.412977281260257,5.55725461111184));
#5649=CARTESIAN_POINT('Ctrl Pts',(3.27280690020258,-0.381974383829492,5.56395850110098));
#5650=CARTESIAN_POINT('Ctrl Pts',(3.27099034153511,-0.350833722259847,5.56990177297914));
#5651=CARTESIAN_POINT('Ctrl Pts',(3.26917378286764,-0.319595685371469,5.57508080114302));
#5652=CARTESIAN_POINT('Ctrl Pts',(3.2652550933095,-0.252208833978631,5.58625302692934));
#5653=CARTESIAN_POINT('Ctrl Pts',(3.26133640375136,-0.184102294733243,5.59390957506827));
#5654=CARTESIAN_POINT('Ctrl Pts',(3.25741771419322,-0.115675333849631,5.59796751668241));
#5655=CARTESIAN_POINT('Ctrl Pts',(3.25350491429959,-0.0473512164897911,
5.60201935934069));
#5656=CARTESIAN_POINT('Ctrl Pts',(3.24959211440596,0.0212918798043963,5.60248330086764));
#5657=CARTESIAN_POINT('Ctrl Pts',(3.24567931451233,0.0898464570696467,5.59932776994969));
#5658=CARTESIAN_POINT('Ctrl Pts',(3.24177110411623,0.158320623613178,5.59617594029471));
#5659=CARTESIAN_POINT('Ctrl Pts',(3.23786289372013,0.226705988457194,5.58941309229315));
#5660=CARTESIAN_POINT('Ctrl Pts',(3.23395468332404,0.29459375043913,5.5790596882954));
#5661=CARTESIAN_POINT('Ctrl Pts',(3.23004891499837,0.362439092315871,5.56871275368881));
#5662=CARTESIAN_POINT('Ctrl Pts',(3.2261431466727,0.429786963122525,5.55477978767467));
#5663=CARTESIAN_POINT('Ctrl Pts',(3.22223737834704,0.496233948595613,5.53733305677324));
#5664=CARTESIAN_POINT('Ctrl Pts',(3.21833271208874,0.562662185118795,5.51989124871191));
#5665=CARTESIAN_POINT('Ctrl Pts',(3.21442804583045,0.628189565578153,5.49893776883435));
#5666=CARTESIAN_POINT('Ctrl Pts',(3.21052337957215,0.692424912524464,5.47459553563127));
#5667=CARTESIAN_POINT('Ctrl Pts',(3.20661847701429,0.75666414681581,5.45025182930376));
#5668=CARTESIAN_POINT('Ctrl Pts',(3.20271357445642,0.819610733474399,5.42251913914844));
#5669=CARTESIAN_POINT('Ctrl Pts',(3.19880867189856,0.880892360436765,5.39156895764098));
#5670=CARTESIAN_POINT('Ctrl Pts',(3.19489961540771,0.942239177187537,5.36058585214172));
#5671=CARTESIAN_POINT('Ctrl Pts',(3.19099055891686,1.00191705989154,5.32637864684416));
#5672=CARTESIAN_POINT('Ctrl Pts',(3.18708150242601,1.0595781643575,5.28916488878023));
#5673=CARTESIAN_POINT('Ctrl Pts',(3.18317010313604,1.11727382662158,5.25192882754416));
#5674=CARTESIAN_POINT('Ctrl Pts',(3.17925870384606,1.17294990653504,5.21168291548388));
#5675=CARTESIAN_POINT('Ctrl Pts',(3.17534730455609,1.22628974279198,5.16868650688894));
#5676=CARTESIAN_POINT('Ctrl Pts',(3.1714291752118,1.27972135694444,5.12561611756641));
#5677=CARTESIAN_POINT('Ctrl Pts',(3.16751104586751,1.33080833887664,5.0797861145422));
#5678=CARTESIAN_POINT('Ctrl Pts',(3.16359291652321,1.37926978606372,5.03149376286202));
#5679=CARTESIAN_POINT('Ctrl Pts',(3.16177735844767,1.40172554595877,5.00911635737697));
#5680=CARTESIAN_POINT('Ctrl Pts',(3.15996180037212,1.42361812047926,4.98621072846779));
#5681=CARTESIAN_POINT('Ctrl Pts',(3.15814624229657,1.44492256927572,4.96280876378078));
#5682=CARTESIAN_POINT('Ctrl Pts',(3.15422851803746,1.49089463538646,4.91231054728197));
#5683=CARTESIAN_POINT('Ctrl Pts',(3.15031079377835,1.53430736323658,4.85929933663352));
#5684=CARTESIAN_POINT('Ctrl Pts',(3.14639306951924,1.57487428716368,4.80406511268991));
#5685=CARTESIAN_POINT('Ctrl Pts',(3.14248123821492,1.61538019121469,4.74891397085298));
#5686=CARTESIAN_POINT('Ctrl Pts',(3.1385694069106,1.65304849789036,4.69154684530576));
#5687=CARTESIAN_POINT('Ctrl Pts',(3.13465757560628,1.68763137962662,4.63228853695296));
#5688=CARTESIAN_POINT('Ctrl Pts',(3.13075033395481,1.72217368614138,4.57309975487636));
#5689=CARTESIAN_POINT('Ctrl Pts',(3.12684309230334,1.7536375103363,4.51202461959078));
#5690=CARTESIAN_POINT('Ctrl Pts',(3.12293585065187,1.78181799743233,4.44941730089291));
#5691=CARTESIAN_POINT('Ctrl Pts',(3.11903105060526,1.8099808747616,4.38684910502059));
#5692=CARTESIAN_POINT('Ctrl Pts',(3.11512625055865,1.83486428347826,4.32275107262859));
#5693=CARTESIAN_POINT('Ctrl Pts',(3.11122145051204,1.85630978619131,4.25750099807221));
#5694=CARTESIAN_POINT('Ctrl Pts',(3.10731775061606,1.87774924678109,4.19226930727672));
#5695=CARTESIAN_POINT('Ctrl Pts',(3.10341405072007,1.89575257068176,4.1258866858309));
#5696=CARTESIAN_POINT('Ctrl Pts',(3.09951035082408,1.91021049363009,4.05874817256462));
#5697=CARTESIAN_POINT('Ctrl Pts',(3.09560641125923,1.92466930422709,3.99160553730843));
#5698=CARTESIAN_POINT('Ctrl Pts',(3.09170247169438,1.93558218067504,3.92370739958937));
#5699=CARTESIAN_POINT('Ctrl Pts',(3.08779853212952,1.94289088911684,3.85545934515353));
#5700=CARTESIAN_POINT('Ctrl Pts',(3.08389042701198,1.95020739604261,3.78713846918396));
#5701=CARTESIAN_POINT('Ctrl Pts',(3.07998232189443,1.95391200778782,3.71846742150226));
#5702=CARTESIAN_POINT('Ctrl Pts',(3.07607421677689,1.95399844922611,3.64985626071567));
#5703=CARTESIAN_POINT('Ctrl Pts',(3.07216376361086,1.95408494259971,3.58120387730907));
#5704=CARTESIAN_POINT('Ctrl Pts',(3.06825331044483,1.95054896473043,3.51261194378154));
#5705=CARTESIAN_POINT('Ctrl Pts',(3.0643428572788,1.94343628034531,3.44448704053023));
#5706=CARTESIAN_POINT('Ctrl Pts',(3.0604256561111,1.93631132208704,3.37624457879108));
#5707=CARTESIAN_POINT('Ctrl Pts',(3.0565084549434,1.92559741588042,3.30847124143886));
#5708=CARTESIAN_POINT('Ctrl Pts',(3.0525912537757,1.91139157959021,3.24156417188939));
#5709=CARTESIAN_POINT('Ctrl Pts',(3.05076706975896,1.90477612677183,3.21040651578396));
#5710=CARTESIAN_POINT('Ctrl Pts',(3.04894288574222,1.8974041141819,3.17943651304369));
#5711=CARTESIAN_POINT('Ctrl Pts',(3.04711870172548,1.88928897332868,3.1486929791557));
#5712=CARTESIAN_POINT('Ctrl Pts',(3.04319933921464,1.87185313432429,3.08263875816405));
#5713=CARTESIAN_POINT('Ctrl Pts',(3.03927997670381,1.85091457533122,3.01736962809996));
#5714=CARTESIAN_POINT('Ctrl Pts',(3.03536061419297,1.82656137564056,2.95328385676861));
#5715=CARTESIAN_POINT('Ctrl Pts',(3.03144714733761,1.8022448089673,2.88929448571348));
#5716=CARTESIAN_POINT('Ctrl Pts',(3.02753368048225,1.77452396902811,2.8264853963439));
#5717=CARTESIAN_POINT('Ctrl Pts',(3.02362021362689,1.74353715277275,2.76524130873555));
#5718=CARTESIAN_POINT('Ctrl Pts',(3.01971134820263,1.712586770632,2.70406923156185));
#5719=CARTESIAN_POINT('Ctrl Pts',(3.01580248277837,1.67837825975927,2.64445893807874));
#5720=CARTESIAN_POINT('Ctrl Pts',(3.0118936173541,1.64109791096867,2.58677500466166));
#5721=CARTESIAN_POINT('Ctrl Pts',(3.00798720177113,1.60384092725407,2.52912722405786));
#5722=CARTESIAN_POINT('Ctrl Pts',(3.00408078618816,1.56351619100125,2.47340382040303));
#5723=CARTESIAN_POINT('Ctrl Pts',(3.00017437060518,1.52035503671783,2.41994322186847));
#5724=CARTESIAN_POINT('Ctrl Pts',(2.99626906576854,1.47720615483419,2.36649782426745));
#5725=CARTESIAN_POINT('Ctrl Pts',(2.9923637609319,1.43122276464048,2.31531433675206));
#5726=CARTESIAN_POINT('Ctrl Pts',(2.98845845609525,1.38267738706865,2.26669926539186));
#5727=CARTESIAN_POINT('Ctrl Pts',(2.98455292455489,1.334129191428,2.21808137191711));
#5728=CARTESIAN_POINT('Ctrl Pts',(2.98064739301452,1.28301906227193,2.17203253660856));
#5729=CARTESIAN_POINT('Ctrl Pts',(2.97674186147416,1.22965609646502,2.12882215047138));
#5730=CARTESIAN_POINT('Ctrl Pts',(2.97283219460914,1.17623662792971,2.0855660115415));
#5731=CARTESIAN_POINT('Ctrl Pts',(2.96892252774413,1.12055994499606,2.04515462963035));
#5732=CARTESIAN_POINT('Ctrl Pts',(2.96501286087911,1.0629671261776,2.00781620279432));
#5733=CARTESIAN_POINT('Ctrl Pts',(2.96110086095524,1.00533993935786,1.97045549458489));
#5734=CARTESIAN_POINT('Ctrl Pts',(2.95718886103137,0.945794766954623,1.93617163639366));
#5735=CARTESIAN_POINT('Ctrl Pts',(2.9532768611075,0.884698047574294,1.90514725143483));
#5736=CARTESIAN_POINT('Ctrl Pts',(2.94935815224908,0.823496549589784,1.87406966080826));
#5737=CARTESIAN_POINT('Ctrl Pts',(2.94543944339066,0.760738643192596,1.84626289884298));
#5738=CARTESIAN_POINT('Ctrl Pts',(2.94152073453225,0.696810697123036,1.82186143588623));
#5739=CARTESIAN_POINT('Ctrl Pts',(2.93971087673963,0.667285540868821,1.8105916071036));
#5740=CARTESIAN_POINT('Ctrl Pts',(2.93790101894702,0.637511017076795,1.80004744746111));
#5741=CARTESIAN_POINT('Ctrl Pts',(2.93609116115441,0.607526056778453,1.79023855389886));
#5742=CARTESIAN_POINT('Ctrl Pts',(2.93217164916576,0.542589235858846,1.76899595900015));
#5743=CARTESIAN_POINT('Ctrl Pts',(2.9282521371771,0.476409137969001,1.75112150272362));
#5744=CARTESIAN_POINT('Ctrl Pts',(2.92433262518844,0.409368097857593,1.73675746444027));
#5745=CARTESIAN_POINT('Ctrl Pts',(2.92041899100293,0.342427594251113,1.72241496684607));
#5746=CARTESIAN_POINT('Ctrl Pts',(2.91650535681742,0.274629187590677,1.71157254128802));
#5747=CARTESIAN_POINT('Ctrl Pts',(2.9125917226319,0.206371096701409,1.70432293834827));
#5748=CARTESIAN_POINT('Ctrl Pts',(2.9086826646809,0.138192820382506,1.6970818124101));
#5749=CARTESIAN_POINT('Ctrl Pts',(2.9047736067299,0.0695564137907122,1.69342521710811));
#5750=CARTESIAN_POINT('Ctrl Pts',(2.90086454877889,0.000869236631294919,
1.69339466162378));
#5751=CARTESIAN_POINT('Ctrl Pts',(2.89695792519361,-0.0677751655906955,
1.69336412516787));
#5752=CARTESIAN_POINT('Ctrl Pts',(2.89305130160832,-0.13646978528588,1.69695514921585));
#5753=CARTESIAN_POINT('Ctrl Pts',(2.88914467802303,-0.204804767933434,1.70415721899295));
#5754=CARTESIAN_POINT('Ctrl Pts',(2.88523915016671,-0.273120583999455,1.71135726873505));
#5755=CARTESIAN_POINT('Ctrl Pts',(2.88133362231038,-0.341076474743408,1.72216630200451));
#5756=CARTESIAN_POINT('Ctrl Pts',(2.87742809445405,-0.408267032846675,1.73652188490983));
#5757=CARTESIAN_POINT('Ctrl Pts',(2.87352232531877,-0.475461741904262,1.75087835468632));
#5758=CARTESIAN_POINT('Ctrl Pts',(2.86961655618349,-0.541890544378382,1.76878170389674));
#5759=CARTESIAN_POINT('Ctrl Pts',(2.86571078704821,-0.607159343224681,1.79011863202934));
#5760=CARTESIAN_POINT('Ctrl Pts',(2.86180086252258,-0.672497582257252,1.81147826075227));
#5761=CARTESIAN_POINT('Ctrl Pts',(2.85789093799696,-0.736672886706858,1.83627860561703));
#5762=CARTESIAN_POINT('Ctrl Pts',(2.85398101347133,-0.799308385936659,1.86435714277121));
#5763=CARTESIAN_POINT('Ctrl Pts',(2.85006874406609,-0.861981449243459,1.89245251932709));
#5764=CARTESIAN_POINT('Ctrl Pts',(2.84615647466084,-0.92311243215019,1.92382977654807));
#5765=CARTESIAN_POINT('Ctrl Pts',(2.84224420525559,-0.982348966787532,1.95828034915175));
#5766=CARTESIAN_POINT('Ctrl Pts',(2.83832521180535,-1.04168731167421,1.99279013219724));
#5767=CARTESIAN_POINT('Ctrl Pts',(2.83440621835512,-1.09912429892442,2.03038350381018));
#5768=CARTESIAN_POINT('Ctrl Pts',(2.83048722490489,-1.15433717467074,2.07080901637421));
#5769=CARTESIAN_POINT('Ctrl Pts',(2.8286793567977,-1.17980738747802,2.08945768109113));
#5770=CARTESIAN_POINT('Ctrl Pts',(2.82687148869051,-1.20480477019509,2.10870848800456));
#5771=CARTESIAN_POINT('Ctrl Pts',(2.82506362058333,-1.22930022257401,2.12853405245248));
#5772=CARTESIAN_POINT('Ctrl Pts',(2.82120048498969,-1.28164323011487,2.17089822900847));
#5773=CARTESIAN_POINT('Ctrl Pts',(2.81733734939605,-1.33191182350578,2.21606720796798));
#5774=CARTESIAN_POINT('Ctrl Pts',(2.81347421380241,-1.37978360123066,2.2638073861763));
#5775=CARTESIAN_POINT('Ctrl Pts',(2.80961772082684,-1.42757306397375,2.31146547568672));
#5776=CARTESIAN_POINT('Ctrl Pts',(2.80576122785128,-1.47297353608629,2.36168563392952));
#5777=CARTESIAN_POINT('Ctrl Pts',(2.80190473487571,-1.51569521873079,2.41419375310542));
#5778=CARTESIAN_POINT('Ctrl Pts',(2.79805193389146,-1.5583760020187,2.46665160393615));
#5779=CARTESIAN_POINT('Ctrl Pts',(2.79419913290721,-1.59838275892305,2.52139268472611));
#5780=CARTESIAN_POINT('Ctrl Pts',(2.79034633192297,-1.6354632437027,2.57810686501829));
#5781=CARTESIAN_POINT('Ctrl Pts',(2.78649581047917,-1.67252178951754,2.63478748991299));
#5782=CARTESIAN_POINT('Ctrl Pts',(2.78264528903538,-1.70665721873714,2.69343847657481));
#5783=CARTESIAN_POINT('Ctrl Pts',(2.77879476759159,-1.73765945873498,2.75371913267879));
#5784=CARTESIAN_POINT('Ctrl Pts',(2.7749451166011,-1.76865469033084,2.81398616166841));
#5785=CARTESIAN_POINT('Ctrl Pts',(2.77109546561061,-1.79651790755939,2.87588167785098));
#5786=CARTESIAN_POINT('Ctrl Pts',(2.76724581462012,-1.8210850163862,2.9390404867932));
#5787=CARTESIAN_POINT('Ctrl Pts',(2.76339335182704,-1.84567006914097,3.00224542721657));
#5788=CARTESIAN_POINT('Ctrl Pts',(2.75954088903397,-1.86695402027117,3.06671503024606));
#5789=CARTESIAN_POINT('Ctrl Pts',(2.75568842624089,-1.88482147805859,3.13206545119962));
#5790=CARTESIAN_POINT('Ctrl Pts',(2.75183446353511,-1.90269589233812,3.19744131559861));
#5791=CARTESIAN_POINT('Ctrl Pts',(2.74798050082933,-1.91715105613517,3.26369818508291));
#5792=CARTESIAN_POINT('Ctrl Pts',(2.74412653812355,-1.92812257189284,3.33044124183343));
#5793=CARTESIAN_POINT('Ctrl Pts',(2.74026661691283,-1.93911105040696,3.39728748817429));
#5794=CARTESIAN_POINT('Ctrl Pts',(2.73640669570212,-1.94660507416329,3.46462091816665));
#5795=CARTESIAN_POINT('Ctrl Pts',(2.73254677449141,-1.950592162525,3.53204189789178));
#5796=CARTESIAN_POINT('Ctrl Pts',(2.73032108038567,-1.95289118330322,3.57091794457406));
#5797=CARTESIAN_POINT('Ctrl Pts',(2.72809538627992,-1.95402516604589,3.60982308596664));
#5798=CARTESIAN_POINT('Ctrl Pts',(2.72586969217418,-1.95399957629683,3.64868125956087));
#5799=CARTESIAN_POINT('Ctrl Pts',(2.6241303079204,-1.95399895847038,3.64941196591101));
#5800=CARTESIAN_POINT('Ctrl Pts',(2.62795723854692,-1.9540679267512,3.58261439099596));
#5801=CARTESIAN_POINT('Ctrl Pts',(2.63178416917345,-1.95070752961312,3.51565940348063));
#5802=CARTESIAN_POINT('Ctrl Pts',(2.63561109979997,-1.94389595297049,3.44893912311788));
#5803=CARTESIAN_POINT('Ctrl Pts',(2.63943211787231,-1.93709490011831,3.38232192465323));
#5804=CARTESIAN_POINT('Ctrl Pts',(2.64325313594464,-1.92685329612979,3.31593922231409));
#5805=CARTESIAN_POINT('Ctrl Pts',(2.64707415401698,-1.91320133873363,3.25018339408295));
#5806=CARTESIAN_POINT('Ctrl Pts',(2.65089193660013,-1.89956094128292,3.18448324532438));
#5807=CARTESIAN_POINT('Ctrl Pts',(2.65470971918328,-1.88251601273262,3.11940942193861));
#5808=CARTESIAN_POINT('Ctrl Pts',(2.65852750176644,-1.86214838250633,3.05534767830098));
#5809=CARTESIAN_POINT('Ctrl Pts',(2.66234348743459,-1.84179033870868,2.991316086592));
#5810=CARTESIAN_POINT('Ctrl Pts',(2.66615947310275,-1.81811284795101,2.92829612128916));
#5811=CARTESIAN_POINT('Ctrl Pts',(2.6699754587709,-1.79124798235692,2.8666597721788));
#5812=CARTESIAN_POINT('Ctrl Pts',(2.67379108292622,-1.76438566184409,2.80502926227567));
#5813=CARTESIAN_POINT('Ctrl Pts',(2.67760670708154,-1.73433677346274,2.74478258014596));
#5814=CARTESIAN_POINT('Ctrl Pts',(2.68142233123687,-1.70128123276077,2.68627108023425));
#5815=CARTESIAN_POINT('Ctrl Pts',(2.68524158368121,-1.66819425944109,2.62770394155307));
#5816=CARTESIAN_POINT('Ctrl Pts',(2.68906083612556,-1.63209518231168,2.57087572752999));
#5817=CARTESIAN_POINT('Ctrl Pts',(2.6928800885699,-1.59320886633476,2.51611134358329));
#5818=CARTESIAN_POINT('Ctrl Pts',(2.6967013208578,-1.55430239227105,2.46131857059595));
#5819=CARTESIAN_POINT('Ctrl Pts',(2.70052255314571,-1.51260612827225,2.40859215759306));
#5820=CARTESIAN_POINT('Ctrl Pts',(2.70434378543361,-1.46838516792302,2.35822380517379));
#5821=CARTESIAN_POINT('Ctrl Pts',(2.70817168727,-1.42408702466089,2.30776754023233));
#5822=CARTESIAN_POINT('Ctrl Pts',(2.71199958910638,-1.37725575526887,2.25967791328992));
#5823=CARTESIAN_POINT('Ctrl Pts',(2.71582749094276,-1.32819236692954,2.21420884303147));
#5824=CARTESIAN_POINT('Ctrl Pts',(2.71790335434256,-1.30158539097325,2.18955105847827));
#5825=CARTESIAN_POINT('Ctrl Pts',(2.71997921774236,-1.27432254066741,2.16566323416872));
#5826=CARTESIAN_POINT('Ctrl Pts',(2.72205508114215,-1.24645540150732,2.14258054887282));
#5827=CARTESIAN_POINT('Ctrl Pts',(2.72597896352972,-1.19377978877061,2.09894870763556));
#5828=CARTESIAN_POINT('Ctrl Pts',(2.72990284591728,-1.1387078737066,2.0580010704438));
#5829=CARTESIAN_POINT('Ctrl Pts',(2.73382672830484,-1.0815439821845,2.02001048943914));
#5830=CARTESIAN_POINT('Ctrl Pts',(2.73774471994961,-1.02446590816368,1.98207694193321));
#5831=CARTESIAN_POINT('Ctrl Pts',(2.74166271159438,-0.965302496310311,1.94709190850392));
#5832=CARTESIAN_POINT('Ctrl Pts',(2.74558070323916,-0.904390978508758,1.91528795943634));
#5833=CARTESIAN_POINT('Ctrl Pts',(2.74949407661558,-0.843551259159038,1.88352149875172));
#5834=CARTESIAN_POINT('Ctrl Pts',(2.75340744999201,-0.780967959127539,1.85492890052282));
#5835=CARTESIAN_POINT('Ctrl Pts',(2.75732082336844,-0.717005575465294,1.82969839777272));
#5836=CARTESIAN_POINT('Ctrl Pts',(2.76123173332034,-0.653083455404191,1.80448377734034));
#5837=CARTESIAN_POINT('Ctrl Pts',(2.76514264327225,-0.587784428964692,1.78262723308188));
#5838=CARTESIAN_POINT('Ctrl Pts',(2.76905355322415,-0.521494381419604,1.76426950956557));
#5839=CARTESIAN_POINT('Ctrl Pts',(2.77296333134663,-0.455223518418963,1.74591709883114));
#5840=CARTESIAN_POINT('Ctrl Pts',(2.77687310946912,-0.38796267590892,1.73106162924765));
#5841=CARTESIAN_POINT('Ctrl Pts',(2.7807828875916,-0.320112646580565,1.71979391487578));
#5842=CARTESIAN_POINT('Ctrl Pts',(2.78469286381552,-0.252259179413235,1.70852562958908));
#5843=CARTESIAN_POINT('Ctrl Pts',(2.78860284003943,-0.183816950128083,1.70084553823986));
#5844=CARTESIAN_POINT('Ctrl Pts',(2.79251281626334,-0.115194905210512,1.69679298827481));
#5845=CARTESIAN_POINT('Ctrl Pts',(2.7964268527083,-0.0465016013759045,1.69273623003643));
#5846=CARTESIAN_POINT('Ctrl Pts',(2.80034088915327,0.022371400493301,1.69231455996694));
#5847=CARTESIAN_POINT('Ctrl Pts',(2.80425492559823,0.0910131025772247,1.69551521608632));
#5848=CARTESIAN_POINT('Ctrl Pts',(2.8081712582225,0.159695073488003,1.69871774987865));
#5849=CARTESIAN_POINT('Ctrl Pts',(2.81208759084677,0.228144986629836,1.70554679127174));
#5850=CARTESIAN_POINT('Ctrl Pts',(2.81600392347104,0.29595769599616,1.71593775321603));
#5851=CARTESIAN_POINT('Ctrl Pts',(2.8199268620398,0.363884789669683,1.72634624230227));
#5852=CARTESIAN_POINT('Ctrl Pts',(2.82384980060857,0.43117205460507,1.74032854398275));
#5853=CARTESIAN_POINT('Ctrl Pts',(2.82777273917733,0.497426112609791,1.75776930373564));
#5854=CARTESIAN_POINT('Ctrl Pts',(2.82954270002263,0.527318777624899,1.765638267609));
#5855=CARTESIAN_POINT('Ctrl Pts',(2.83131266086794,0.557001347279425,1.77421058611092));
#5856=CARTESIAN_POINT('Ctrl Pts',(2.83308262171324,0.586438997343527,1.78347244674039));
#5857=CARTESIAN_POINT('Ctrl Pts',(2.83700779777913,0.651721774515743,1.80401212916604));
#5858=CARTESIAN_POINT('Ctrl Pts',(2.84093297384501,0.71604823677107,1.82802469709653));
#5859=CARTESIAN_POINT('Ctrl Pts',(2.8448581499109,0.779023915909599,1.8554017957428));
#5860=CARTESIAN_POINT('Ctrl Pts',(2.84877757921274,0.841907393739763,1.88273881218038));
#5861=CARTESIAN_POINT('Ctrl Pts',(2.85269700851457,0.90344356815947,1.91343038786905));
#5862=CARTESIAN_POINT('Ctrl Pts',(2.85661643781641,0.96325406217776,1.94731870182579));
#5863=CARTESIAN_POINT('Ctrl Pts',(2.86053145588644,1.02299724079535,1.98116887522759));
#5864=CARTESIAN_POINT('Ctrl Pts',(2.86444647395646,1.08101817229185,2.01820840059012));
#5865=CARTESIAN_POINT('Ctrl Pts',(2.86836149202648,1.13696100915589,2.05823253076484));
#5866=CARTESIAN_POINT('Ctrl Pts',(2.87227417452959,1.192870472422,2.09823278390181));
#5867=CARTESIAN_POINT('Ctrl Pts',(2.8761868570327,1.24670390311263,2.14121382493048));
#5868=CARTESIAN_POINT('Ctrl Pts',(2.88009953953581,1.29813382908859,2.18692722737232));
#5869=CARTESIAN_POINT('Ctrl Pts',(2.8840112156736,1.34955052698037,2.23262887205398));
#5870=CARTESIAN_POINT('Ctrl Pts',(2.8879228918114,1.39856458168815,2.28106115747737));
#5871=CARTESIAN_POINT('Ctrl Pts',(2.89183456794919,1.44488245081876,2.33193610584286));
#5872=CARTESIAN_POINT('Ctrl Pts',(2.89574656539129,1.49120412448991,2.38281523306647));
#5873=CARTESIAN_POINT('Ctrl Pts',(2.89965856283338,1.53482884503913,2.43613705771197));
#5874=CARTESIAN_POINT('Ctrl Pts',(2.90357056027547,1.57550194059927,2.49157889685046));
#5875=CARTESIAN_POINT('Ctrl Pts',(2.90748679134103,1.61621905320547,2.54708073599519));
#5876=CARTESIAN_POINT('Ctrl Pts',(2.91140302240658,1.65397787595406,2.60470677256874));
#5877=CARTESIAN_POINT('Ctrl Pts',(2.91531925347213,1.6885664370755,2.66410438515369));
#5878=CARTESIAN_POINT('Ctrl Pts',(2.91923788309565,1.72317618251101,2.72353837675064));
#5879=CARTESIAN_POINT('Ctrl Pts',(2.92315651271918,1.75461157795443,2.78474566821742));
#5880=CARTESIAN_POINT('Ctrl Pts',(2.9270751423427,1.78270739879702,2.84735051306993));
#5881=CARTESIAN_POINT('Ctrl Pts',(2.93100051228645,1.81085154643947,2.91006304268541));
#5882=CARTESIAN_POINT('Ctrl Pts',(2.9349258822302,1.83564447823696,2.97417746692774));
#5883=CARTESIAN_POINT('Ctrl Pts',(2.93885125217395,1.85697002178265,3.03930044742808));
#5884=CARTESIAN_POINT('Ctrl Pts',(2.94060422221074,1.86649346527703,3.06838270850395));
#5885=CARTESIAN_POINT('Ctrl Pts',(2.94235719224753,1.87532608795664,3.09766593971382));
#5886=CARTESIAN_POINT('Ctrl Pts',(2.94411016228432,1.88346084202322,3.1271144892676));
#5887=CARTESIAN_POINT('Ctrl Pts',(2.9480236060212,1.90162139336457,3.19285733677376));
#5888=CARTESIAN_POINT('Ctrl Pts',(2.95193704975808,1.91637244034916,3.25968545217464));
#5889=CARTESIAN_POINT('Ctrl Pts',(2.95585049349497,1.92758891674177,3.32721175786014));
#5890=CARTESIAN_POINT('Ctrl Pts',(2.95975797103281,1.93878829317455,3.39463511703428));
#5891=CARTESIAN_POINT('Ctrl Pts',(2.96366544857066,1.94646371236138,3.46275407167435));
#5892=CARTESIAN_POINT('Ctrl Pts',(2.9675729261085,1.950540275588,3.53116782198833));
#5893=CARTESIAN_POINT('Ctrl Pts',(2.97147572681058,1.95461195960123,3.59949968830653));
#5894=CARTESIAN_POINT('Ctrl Pts',(2.97537852751266,1.95509331260623,3.6681251596545));
#5895=CARTESIAN_POINT('Ctrl Pts',(2.97928132821474,1.95196102673349,3.7366365554038));
#5896=CARTESIAN_POINT('Ctrl Pts',(2.98318163565292,1.94883074188923,3.80510418335578));
#5897=CARTESIAN_POINT('Ctrl Pts',(2.98708194309109,1.94209141961315,3.8734573886953));
#5898=CARTESIAN_POINT('Ctrl Pts',(2.99098225052927,1.93177183353233,3.94128829804409));
#5899=CARTESIAN_POINT('Ctrl Pts',(2.9948814128957,1.92145527712716,4.00909929325557));
#5900=CARTESIAN_POINT('Ctrl Pts',(2.99878057526213,1.90756061748983,4.07638780947079));
#5901=CARTESIAN_POINT('Ctrl Pts',(3.00267973762855,1.89016829610894,4.14275273498043));
#5902=CARTESIAN_POINT('Ctrl Pts',(3.00657910142912,1.87277507622552,4.20912108896016));
#5903=CARTESIAN_POINT('Ctrl Pts',(3.01047846522969,1.85188396342224,4.27456528104707));
#5904=CARTESIAN_POINT('Ctrl Pts',(3.01437782903025,1.82762570351886,4.33869779377652));
#5905=CARTESIAN_POINT('Ctrl Pts',(3.01828133160984,1.80334169593394,4.40289837666106));
#5906=CARTESIAN_POINT('Ctrl Pts',(3.02218483418944,1.77568358378569,4.46578403956246));
#5907=CARTESIAN_POINT('Ctrl Pts',(3.02608833676903,1.7448305018353,4.52698671464874));
#5908=CARTESIAN_POINT('Ctrl Pts',(3.02999416525936,1.71395903600712,4.58822585748564));
#5909=CARTESIAN_POINT('Ctrl Pts',(3.03389999374968,1.67988905689783,4.64777958873476));
#5910=CARTESIAN_POINT('Ctrl Pts',(3.03780582224,1.64284456515422,4.70530643756262));
#5911=CARTESIAN_POINT('Ctrl Pts',(3.04171841300615,1.60573593719169,4.7629328843171));
#5912=CARTESIAN_POINT('Ctrl Pts',(3.04563100377231,1.5656428070228,4.81852504529772));
#5913=CARTESIAN_POINT('Ctrl Pts',(3.04954359453846,1.52283064471812,4.87177301575495));
#5914=CARTESIAN_POINT('Ctrl Pts',(3.05140829731077,1.50242678382146,4.8971504814972));
#5915=CARTESIAN_POINT('Ctrl Pts',(3.05327300008308,1.48140588582222,4.92199601484909));
#5916=CARTESIAN_POINT('Ctrl Pts',(3.05513770285539,1.45979955695045,4.94627908730408));
#5917=CARTESIAN_POINT('Ctrl Pts',(3.05905724628881,1.41438376966934,4.9973213008931));
#5918=CARTESIAN_POINT('Ctrl Pts',(3.06297678972224,1.36619821726603,5.04607926715039));
#5919=CARTESIAN_POINT('Ctrl Pts',(3.06689633315566,1.31550159430471,5.09223755851262));
#5920=CARTESIAN_POINT('Ctrl Pts',(3.07080998965572,1.26488111481424,5.13832652272232));
#5921=CARTESIAN_POINT('Ctrl Pts',(3.07472364615578,1.21175741053974,5.18182323319347));
#5922=CARTESIAN_POINT('Ctrl Pts',(3.07863730265584,1.15642783819774,5.22244705630793));
#5923=CARTESIAN_POINT('Ctrl Pts',(3.08254636936972,1.10116315425515,5.26302323736141));
#5924=CARTESIAN_POINT('Ctrl Pts',(3.08645543608361,1.04369813440837,5.30073293304372));
#5925=CARTESIAN_POINT('Ctrl Pts',(3.09036450279749,0.984363832719194,5.33533517957511));
#5926=CARTESIAN_POINT('Ctrl Pts',(3.09427112673113,0.92506660910272,5.36991580312324));
#5927=CARTESIAN_POINT('Ctrl Pts',(3.09817775066478,0.863902844490097,5.40139258262384));
#5928=CARTESIAN_POINT('Ctrl Pts',(3.10208437459842,0.801231943442729,5.42956824567119));
#5929=CARTESIAN_POINT('Ctrl Pts',(3.10598989441529,0.738578754874032,5.45773594551995));
#5930=CARTESIAN_POINT('Ctrl Pts',(3.10989541423216,0.674419723535876,5.48260417968945));
#5931=CARTESIAN_POINT('Ctrl Pts',(3.11380093404903,0.609136553962107,5.50402277212586));
#5932=CARTESIAN_POINT('Ctrl Pts',(3.1177066867749,0.543849491171074,5.52544264187822));
#5933=CARTESIAN_POINT('Ctrl Pts',(3.12161243950076,0.477438624815858,5.54341231069807));
#5934=CARTESIAN_POINT('Ctrl Pts',(3.12551819222662,0.410301499896432,5.55783124535417));
#5935=CARTESIAN_POINT('Ctrl Pts',(3.12942808785887,0.343093161348362,5.5722654744492));
#5936=CARTESIAN_POINT('Ctrl Pts',(3.13333798349113,0.27515750827182,5.58314134960697));
#5937=CARTESIAN_POINT('Ctrl Pts',(3.13724787912339,0.206901985992685,5.59040953981376));
#5938=CARTESIAN_POINT('Ctrl Pts',(3.14116011246107,0.138605654106479,5.59768207563209));
#5939=CARTESIAN_POINT('Ctrl Pts',(3.14507234579874,0.0699895632146808,5.60134260730777));
#5940=CARTESIAN_POINT('Ctrl Pts',(3.14898457913642,0.0014631717957429,5.60139392046606));
#5941=CARTESIAN_POINT('Ctrl Pts',(3.15290352589339,-0.0671808113816727,
5.60144532167808));
#5942=CARTESIAN_POINT('Ctrl Pts',(3.15682247265035,-0.135734297356499,5.59787516888501));
#5943=CARTESIAN_POINT('Ctrl Pts',(3.16074141940731,-0.203791822251691,5.59073820864051));
#5944=CARTESIAN_POINT('Ctrl Pts',(3.16254936074703,-0.235189036954434,5.5874456899445));
#5945=CARTESIAN_POINT('Ctrl Pts',(3.16435730208675,-0.266480827607967,5.58339477144296));
#5946=CARTESIAN_POINT('Ctrl Pts',(3.16616524342647,-0.297628256975112,5.57859446327402));
#5947=CARTESIAN_POINT('Ctrl Pts',(3.1700845073386,-0.365149803826313,5.56818833218987));
#5948=CARTESIAN_POINT('Ctrl Pts',(3.17400377125072,-0.432257843245543,5.5542162717806));
#5949=CARTESIAN_POINT('Ctrl Pts',(3.17792303516284,-0.498547063155574,5.53672419753151));
#5950=CARTESIAN_POINT('Ctrl Pts',(3.18183642540956,-0.564736937702167,5.5192583380497));
#5951=CARTESIAN_POINT('Ctrl Pts',(3.18574981565628,-0.630109956738539,5.49828305905177));
#5952=CARTESIAN_POINT('Ctrl Pts',(3.189663205903,-0.694269029376674,5.47389563577552));
#5953=CARTESIAN_POINT('Ctrl Pts',(3.19357202746939,-0.758353199622102,5.44953668355224));
#5954=CARTESIAN_POINT('Ctrl Pts',(3.19748084903578,-0.821225780809679,5.42177367228869));
#5955=CARTESIAN_POINT('Ctrl Pts',(3.20138967060217,-0.8825046924029,5.39075371636984));
#5956=CARTESIAN_POINT('Ctrl Pts',(3.20529606267586,-0.943745516642773,5.35975304062406));
#5957=CARTESIAN_POINT('Ctrl Pts',(3.20920245474956,-1.00339419865752,5.32549965745876));
#5958=CARTESIAN_POINT('Ctrl Pts',(3.21310884682325,-1.06108995211075,5.28818821325294));
#5959=CARTESIAN_POINT('Ctrl Pts',(3.21701414846881,-1.11876960040304,5.25088718414316));
#5960=CARTESIAN_POINT('Ctrl Pts',(3.22091945011436,-1.17449698980819,5.21053005545042));
#5961=CARTESIAN_POINT('Ctrl Pts',(3.22482475175992,-1.22793877375843,5.1673557730218));
#5962=CARTESIAN_POINT('Ctrl Pts',(3.2287303004185,-1.28138393793846,5.12417875978997));
#5963=CARTESIAN_POINT('Ctrl Pts',(3.23263584907708,-1.33254282891501,5.07818454995117));
#5964=CARTESIAN_POINT('Ctrl Pts',(3.23654139773567,-1.38111518643624,5.0296523464655));
#5965=CARTESIAN_POINT('Ctrl Pts',(3.24045111216644,-1.4297393526517,4.98106837711507));
#5966=CARTESIAN_POINT('Ctrl Pts',(3.24436082659722,-1.47577113126628,4.92994135975682));
#5967=CARTESIAN_POINT('Ctrl Pts',(3.248270541028,-1.51894788216773,4.87658661406831));
#5968=CARTESIAN_POINT('Ctrl Pts',(3.25218260598123,-1.56215059095551,4.82319979147743));
#5969=CARTESIAN_POINT('Ctrl Pts',(3.25609467093447,-1.6024945673085,4.76758297297988));
#5970=CARTESIAN_POINT('Ctrl Pts',(3.2600067358877,-1.6397598443748,4.7100814648995));
#5971=CARTESIAN_POINT('Ctrl Pts',(3.26392553588139,-1.67708927762243,4.65248096179023));
#5972=CARTESIAN_POINT('Ctrl Pts',(3.26784433587508,-1.71132918811501,4.59298971906679));
#5973=CARTESIAN_POINT('Ctrl Pts',(3.27176313586877,-1.74230541245399,4.53197790116826));
#5974=CARTESIAN_POINT('Ctrl Pts',(3.27357301857837,-1.75661166256368,4.50379982765771));
#5975=CARTESIAN_POINT('Ctrl Pts',(3.27538290128796,-1.77022243794753,4.47529769357849));
#5976=CARTESIAN_POINT('Ctrl Pts',(3.27719278399755,-1.7831241210405,4.44650920908367));
#5977=CARTESIAN_POINT('Ctrl Pts',(3.2814779271289,-1.8136706080563,4.37834856202015));
#5978=CARTESIAN_POINT('Ctrl Pts',(3.28576307026025,-1.84034342649034,4.30834888308732));
#5979=CARTESIAN_POINT('Ctrl Pts',(3.29004821339159,-1.8629392632888,4.23694794448174));
#5980=CARTESIAN_POINT('Ctrl Pts',(3.29432122677543,-1.88547113914435,4.16574911706143));
#5981=CARTESIAN_POINT('Ctrl Pts',(3.29859424015927,-1.90394890645761,4.09315724465676));
#5982=CARTESIAN_POINT('Ctrl Pts',(3.3028672535431,-1.91821713524752,4.01962963863027));
#5983=CARTESIAN_POINT('Ctrl Pts',(3.30712062229899,-1.93241976769572,3.94644006628971));
#5984=CARTESIAN_POINT('Ctrl Pts',(3.31137399105488,-1.94245134242051,3.87232365766614));
#5985=CARTESIAN_POINT('Ctrl Pts',(3.31562735981078,-1.94820666808604,3.79774997508393));
#5986=CARTESIAN_POINT('Ctrl Pts',(3.31846167581925,-1.95204184265095,3.74805633352957));
#5987=CARTESIAN_POINT('Ctrl Pts',(3.32129599182773,-1.95397914847566,3.698160016538));
#5988=CARTESIAN_POINT('Ctrl Pts',(3.3241303078362,-1.95399983251307,3.64820350405597));
#5989=CARTESIAN_POINT('Origin',(0.,0.,3.64739446828387));
#5990=CARTESIAN_POINT('',(4.12586969212423,-1.95399924590383,3.64567778332306));
#5991=CARTESIAN_POINT('',(4.02413030792419,-1.95399922086733,3.64564951846532));
#5992=CARTESIAN_POINT('',(0.,-1.954,3.64739446828387));
#5993=CARTESIAN_POINT('Ctrl Pts',(4.12586969212423,-1.95399924590383,3.64567778332306));
#5994=CARTESIAN_POINT('Ctrl Pts',(4.12199411980701,-1.95405905160708,3.71375101849607));
#5995=CARTESIAN_POINT('Ctrl Pts',(4.11811854748978,-1.95055728305734,3.78189644852607));
#5996=CARTESIAN_POINT('Ctrl Pts',(4.11424297517256,-1.94349799785706,3.84970989608311));
#5997=CARTESIAN_POINT('Ctrl Pts',(4.11036920668271,-1.93644199829586,3.91749178088173));
#5998=CARTESIAN_POINT('Ctrl Pts',(4.10649543819285,-1.92583181766029,3.98494149260619));
#5999=CARTESIAN_POINT('Ctrl Pts',(4.102621669703,-1.91172349358431,4.05165834754814));
#6000=CARTESIAN_POINT('Ctrl Pts',(4.09874832349887,-1.89761670747941,4.11836792957855));
#6001=CARTESIAN_POINT('Ctrl Pts',(4.09487497729474,-1.88001263979045,4.18434432418101));
#6002=CARTESIAN_POINT('Ctrl Pts',(4.09100163109061,-1.85901836975748,4.24919734373748));
#6003=CARTESIAN_POINT('Ctrl Pts',(4.08712457443049,-1.83800398835026,4.31411248897616));
#6004=CARTESIAN_POINT('Ctrl Pts',(4.08324751777036,-1.81359307231316,4.37790163250603));
#6005=CARTESIAN_POINT('Ctrl Pts',(4.07937046111024,-1.78594218915509,4.44019109857181));
#6006=CARTESIAN_POINT('Ctrl Pts',(4.07549157612676,-1.75827826652926,4.50250993879827));
#6007=CARTESIAN_POINT('Ctrl Pts',(4.07161269114329,-1.7273715618897,4.56332724688191));
#6008=CARTESIAN_POINT('Ctrl Pts',(4.06773380615981,-1.69342499635027,4.62229332546655));
#6009=CARTESIAN_POINT('Ctrl Pts',(4.06384772938108,-1.65941549088091,4.68136873236748));
#6010=CARTESIAN_POINT('Ctrl Pts',(4.05996165260234,-1.62235514002231,4.73858563361905));
#6011=CARTESIAN_POINT('Ctrl Pts',(4.05607557582361,-1.58249024166121,4.79362334379131));
#6012=CARTESIAN_POINT('Ctrl Pts',(4.05283923950414,-1.54929063553293,4.83945891280168));
#6013=CARTESIAN_POINT('Ctrl Pts',(4.04960290318466,-1.5141467635391,4.8837835390167));
#6014=CARTESIAN_POINT('Ctrl Pts',(4.04636656686519,-1.47722071628238,4.92643119777453));
#6015=CARTESIAN_POINT('Ctrl Pts',(4.04244807472578,-1.43251138708061,4.97806814125327));
#6016=CARTESIAN_POINT('Ctrl Pts',(4.03852958258636,-1.38500289026933,5.02746012816018));
#6017=CARTESIAN_POINT('Ctrl Pts',(4.03461109044695,-1.33494940519814,5.07428832753239));
#6018=CARTESIAN_POINT('Ctrl Pts',(4.03069848988681,-1.28497117715565,5.12104611919694));
#6019=CARTESIAN_POINT('Ctrl Pts',(4.02678588932668,-1.23245591134374,5.16524744040475));
#6020=CARTESIAN_POINT('Ctrl Pts',(4.02287328876654,-1.17769692864366,5.20660771356602));
#6021=CARTESIAN_POINT('Ctrl Pts',(4.018965279537,-1.12300220412392,5.24791945156902));
#6022=CARTESIAN_POINT('Ctrl Pts',(4.01505727030746,-1.06606938237395,5.28639646773815));
#6023=CARTESIAN_POINT('Ctrl Pts',(4.01114926107791,-1.00722602659854,5.32179338471404));
#6024=CARTESIAN_POINT('Ctrl Pts',(4.00724369493527,-0.948419456670685,5.35716817335318));
#6025=CARTESIAN_POINT('Ctrl Pts',(4.00333812879263,-0.887705142448082,5.38946642953741));
#6026=CARTESIAN_POINT('Ctrl Pts',(3.99943256264998,-0.825439595234824,5.4184860736557));
#6027=CARTESIAN_POINT('Ctrl Pts',(3.99552809927701,-0.763191629226074,5.44749752383175));
#6028=CARTESIAN_POINT('Ctrl Pts',(3.99162363590404,-0.699393745279336,5.47323199209042));
#6029=CARTESIAN_POINT('Ctrl Pts',(3.98771917253107,-0.634425395958315,5.4955341862065));
#6030=CARTESIAN_POINT('Ctrl Pts',(3.98381447324754,-0.569453121201594,5.51783772783764));
#6031=CARTESIAN_POINT('Ctrl Pts',(3.97990977396401,-0.503310706622887,5.5367084263743));
#6032=CARTESIAN_POINT('Ctrl Pts',(3.97600507468047,-0.436394118018742,5.55204041274668));
#6033=CARTESIAN_POINT('Ctrl Pts',(3.97209622064834,-0.369406327618353,5.56738871293591));
#6034=CARTESIAN_POINT('Ctrl Pts',(3.96818736661621,-0.301643199518616,5.57919067659121));
#6035=CARTESIAN_POINT('Ctrl Pts',(3.96427851258407,-0.233511292379936,5.58739149826383));
#6036=CARTESIAN_POINT('Ctrl Pts',(3.96036731558006,-0.165338546892934,5.59559723551896));
#6037=CARTESIAN_POINT('Ctrl Pts',(3.95645611857605,-0.0967970731618409,
5.60019750197601));
#6038=CARTESIAN_POINT('Ctrl Pts',(3.95254492157203,-0.0282961421001321,
5.60118957738366));
#6039=CARTESIAN_POINT('Ctrl Pts',(3.94862699211985,0.0403227014490757,5.60218336047727));
#6040=CARTESIAN_POINT('Ctrl Pts',(3.94470906266767,0.108900371926006,5.59955657561392));
#6041=CARTESIAN_POINT('Ctrl Pts',(3.94079113321549,0.177030896039916,5.59335851261956));
#6042=CARTESIAN_POINT('Ctrl Pts',(3.9389737642417,0.208633889969279,5.5904834819379));
#6043=CARTESIAN_POINT('Ctrl Pts',(3.93715639526791,0.240140795167076,5.58684076103467));
#6044=CARTESIAN_POINT('Ctrl Pts',(3.93533902629411,0.271511933329578,5.58243898199916));
#6045=CARTESIAN_POINT('Ctrl Pts',(3.93142052909791,0.339152417295069,5.57294814163727));
#6046=CARTESIAN_POINT('Ctrl Pts',(3.92750203190172,0.4064284310436,5.5598876511501));
#6047=CARTESIAN_POINT('Ctrl Pts',(3.92358353470552,0.472934213080639,5.54329774379605));
#6048=CARTESIAN_POINT('Ctrl Pts',(3.91967092903786,0.539340002520195,5.52673277965561));
#6049=CARTESIAN_POINT('Ctrl Pts',(3.9157583233702,0.604977385279625,5.50664904841392));
#6050=CARTESIAN_POINT('Ctrl Pts',(3.91184571770254,0.669448099006128,5.48313825289464));
#6051=CARTESIAN_POINT('Ctrl Pts',(3.90793770331604,0.733843159012707,5.45965504632291));
#6052=CARTESIAN_POINT('Ctrl Pts',(3.90402968892955,0.797073809110116,5.43275293001398));
#6053=CARTESIAN_POINT('Ctrl Pts',(3.90012167454305,0.858756100670228,5.40257364989516));
#6054=CARTESIAN_POINT('Ctrl Pts',(3.89621610321588,0.920399832111779,5.37241323607637));
#6055=CARTESIAN_POINT('Ctrl Pts',(3.89231053188872,0.980496684386062,5.33897993808273));
#6056=CARTESIAN_POINT('Ctrl Pts',(3.88840496056155,1.03868333862023,5.30246332548369));
#6057=CARTESIAN_POINT('Ctrl Pts',(3.88450049198455,1.09685356367234,5.26595702346334));
#6058=CARTESIAN_POINT('Ctrl Pts',(3.88059602340755,1.15311424506722,5.22636939640863));
#6059=CARTESIAN_POINT('Ctrl Pts',(3.87669155483054,1.20712888640244,5.1839346895644));
#6060=CARTESIAN_POINT('Ctrl Pts',(3.87278685033151,1.26114679149643,5.14149741866265));
#6061=CARTESIAN_POINT('Ctrl Pts',(3.86888214583249,1.31291800198357,5.09621303225256));
#6062=CARTESIAN_POINT('Ctrl Pts',(3.86497744133346,1.36213854850416,5.04835648585572));
#6063=CARTESIAN_POINT('Ctrl Pts',(3.86106858210453,1.41141146725322,5.00044901856996));
#6064=CARTESIAN_POINT('Ctrl Pts',(3.85715972287561,1.45812795256836,4.94996427289987));
#6065=CARTESIAN_POINT('Ctrl Pts',(3.85325086364668,1.50202115528847,4.89721383485885));
#6066=CARTESIAN_POINT('Ctrl Pts',(3.84933966144904,1.54594066757743,4.84443177822555));
#6067=CARTESIAN_POINT('Ctrl Pts',(3.8454284592514,1.58703323512623,4.78938172056141));
#6068=CARTESIAN_POINT('Ctrl Pts',(3.84151725705375,1.62507426724836,4.73240581657807));
#6069=CARTESIAN_POINT('Ctrl Pts',(3.83759932246746,1.66318077975223,4.67533183944228));
#6070=CARTESIAN_POINT('Ctrl Pts',(3.83368138788116,1.6982250226033,4.61632582249884));
#6071=CARTESIAN_POINT('Ctrl Pts',(3.82976345329487,1.73002786493561,4.55575540235487));
#6072=CARTESIAN_POINT('Ctrl Pts',(3.82794613077092,1.74477952053959,4.52765998973685));
#6073=CARTESIAN_POINT('Ctrl Pts',(3.82612880824698,1.75883445140535,4.49922828152488));
#6074=CARTESIAN_POINT('Ctrl Pts',(3.82431148572303,1.77217835395763,4.47049827811835));
#6075=CARTESIAN_POINT('Ctrl Pts',(3.82039300905922,1.80095022580008,4.40855118484431));
#6076=CARTESIAN_POINT('Ctrl Pts',(3.8164745323954,1.8265270178764,4.34497116695154));
#6077=CARTESIAN_POINT('Ctrl Pts',(3.81255605573159,1.84872211032279,4.28012075887377));
#6078=CARTESIAN_POINT('Ctrl Pts',(3.80864347063613,1.87088383166211,4.21536785567986));
#6079=CARTESIAN_POINT('Ctrl Pts',(3.80473088554067,1.88967378643479,4.14934881470658));
#6080=CARTESIAN_POINT('Ctrl Pts',(3.80081830044521,1.90495264280254,4.08244783130918));
#6081=CARTESIAN_POINT('Ctrl Pts',(3.79691030659027,1.92021357012777,4.01562535317073));
#6082=CARTESIAN_POINT('Ctrl Pts',(3.79300231273533,1.93197147273745,3.9479234651545));
#6083=CARTESIAN_POINT('Ctrl Pts',(3.7890943188804,1.94013681071575,3.87974152702515));
#6084=CARTESIAN_POINT('Ctrl Pts',(3.78518876804767,1.94829704425869,3.81160221178502));
#6085=CARTESIAN_POINT('Ctrl Pts',(3.78128321721494,1.95286910989961,3.74298392892463));
#6086=CARTESIAN_POINT('Ctrl Pts',(3.77737766638221,1.95381482691184,3.6742946939236));
#6087=CARTESIAN_POINT('Ctrl Pts',(3.77347321823199,1.95476027691292,3.60562485245269));
#6088=CARTESIAN_POINT('Ctrl Pts',(3.76956877008177,1.95208140407651,3.53688459010406));
#6089=CARTESIAN_POINT('Ctrl Pts',(3.76566432193155,1.94579210753576,3.4684836685776));
#6090=CARTESIAN_POINT('Ctrl Pts',(3.76175963776104,1.93950243081285,3.40007861227866));
#6091=CARTESIAN_POINT('Ctrl Pts',(3.75785495359054,1.92960194468172,3.33201342699205));
#6092=CARTESIAN_POINT('Ctrl Pts',(3.75395026942003,1.91615639730594,3.26469267698481));
#6093=CARTESIAN_POINT('Ctrl Pts',(3.75004143023388,1.90269654238124,3.19730029025668));
#6094=CARTESIAN_POINT('Ctrl Pts',(3.74613259104772,1.88568419438441,3.1306544028623));
#6095=CARTESIAN_POINT('Ctrl Pts',(3.74222375186156,1.86523601993753,3.06514830906286));
#6096=CARTESIAN_POINT('Ctrl Pts',(3.73831256957263,1.84477558809861,2.99960294848809));
#6097=CARTESIAN_POINT('Ctrl Pts',(3.73440138728369,1.82087540201003,2.93519920237402));
#6098=CARTESIAN_POINT('Ctrl Pts',(3.73049020499476,1.79370074809955,2.87231148803781));
#6099=CARTESIAN_POINT('Ctrl Pts',(3.72657228990375,1.76647931509443,2.80931551729655));
#6100=CARTESIAN_POINT('Ctrl Pts',(3.72265437481273,1.73597238288057,2.74784122711538));
#6101=CARTESIAN_POINT('Ctrl Pts',(3.71873645972171,1.70239132559535,2.68823870693032));
#6102=CARTESIAN_POINT('Ctrl Pts',(3.71691895486513,1.68681320986613,2.66058934052384));
#6103=CARTESIAN_POINT('Ctrl Pts',(3.71510145000855,1.67057415673778,2.63334236908991));
#6104=CARTESIAN_POINT('Ctrl Pts',(3.71328394515196,1.65369831032235,2.60653045294036));
#6105=CARTESIAN_POINT('Ctrl Pts',(3.709365444375,1.61731435401475,2.5487245472872));
#6106=CARTESIAN_POINT('Ctrl Pts',(3.70544694359804,1.57782384186816,2.49271435131038));
#6107=CARTESIAN_POINT('Ctrl Pts',(3.70152844282107,1.53542980063071,2.43885347711512));
#6108=CARTESIAN_POINT('Ctrl Pts',(3.69761583371803,1.49309950108459,2.38507358560323));
#6109=CARTESIAN_POINT('Ctrl Pts',(3.69370322461499,1.44787463843252,2.3334369855227));
#6110=CARTESIAN_POINT('Ctrl Pts',(3.68979061551194,1.40000211194106,2.28426935056335));
#6111=CARTESIAN_POINT('Ctrl Pts',(3.68588259791834,1.35218576462613,2.23515941461106));
#6112=CARTESIAN_POINT('Ctrl Pts',(3.68197458032474,1.30172826565825,2.18851304019558));
#6113=CARTESIAN_POINT('Ctrl Pts',(3.67806656273114,1.24891629228578,2.1446223315768));
#6114=CARTESIAN_POINT('Ctrl Pts',(3.67416098833998,1.19613733574069,2.10075906241648));
#6115=CARTESIAN_POINT('Ctrl Pts',(3.67025541394882,1.1410072020901,2.05964835518222));
#6116=CARTESIAN_POINT('Ctrl Pts',(3.66634983955766,1.08384773311687,2.0215438935331));
#6117=CARTESIAN_POINT('Ctrl Pts',(3.66244536806308,1.02670440542709,1.9834501922169));
#6118=CARTESIAN_POINT('Ctrl Pts',(3.65854089656851,0.967533289053315,1.94836132382126));
#6119=CARTESIAN_POINT('Ctrl Pts',(3.65463642507394,0.906685980489135,1.91648819329829));
#6120=CARTESIAN_POINT('Ctrl Pts',(3.65073171780722,0.845834997650355,1.88461313811117));
#6121=CARTESIAN_POINT('Ctrl Pts',(3.6468270105405,0.783308058479606,1.85595443221992));
#6122=CARTESIAN_POINT('Ctrl Pts',(3.64292230327378,0.719480558858603,1.83067662408667));
#6123=CARTESIAN_POINT('Ctrl Pts',(3.63901344151935,0.655585148752814,1.80537192114766));
#6124=CARTESIAN_POINT('Ctrl Pts',(3.63510457976491,0.590386874765151,1.78345547613772));
#6125=CARTESIAN_POINT('Ctrl Pts',(3.63119571801047,0.52427932807126,1.76504296387319));
#6126=CARTESIAN_POINT('Ctrl Pts',(3.62728451342184,0.458132158840093,1.74661941579672));
#6127=CARTESIAN_POINT('Ctrl Pts',(3.62337330883321,0.391075112365833,1.7317040869153));
#6128=CARTESIAN_POINT('Ctrl Pts',(3.61946210424458,0.323512339794136,1.72036157650415));
#6129=CARTESIAN_POINT('Ctrl Pts',(3.61554416749687,0.255833274831545,1.70899954280222));
#6130=CARTESIAN_POINT('Ctrl Pts',(3.61162623074917,0.187647234771641,1.70122265691404));
#6131=CARTESIAN_POINT('Ctrl Pts',(3.60770829400146,0.119362978637942,1.69704360771271));
#6132=CARTESIAN_POINT('Ctrl Pts',(3.60589099752793,0.0876899972041078,1.69510519679254));
#6133=CARTESIAN_POINT('Ctrl Pts',(3.60407370105441,0.0559958742510644,1.69394011591223));
#6134=CARTESIAN_POINT('Ctrl Pts',(3.60225640458088,0.0243211323379382,1.69354583481151));
#6135=CARTESIAN_POINT('Ctrl Pts',(3.59833787824393,-0.0439771955413948,
1.69269567035028));
#6136=CARTESIAN_POINT('Ctrl Pts',(3.59441935190697,-0.112455204635342,1.69542926853146));
#6137=CARTESIAN_POINT('Ctrl Pts',(3.59050082557002,-0.180705710999077,1.70176823336301));
#6138=CARTESIAN_POINT('Ctrl Pts',(3.58658819053925,-0.248853606177836,1.70809766788149));
#6139=CARTESIAN_POINT('Ctrl Pts',(3.58267555550849,-0.316774191731215,1.71802166608975));
#6140=CARTESIAN_POINT('Ctrl Pts',(3.57876292047773,-0.384059911532484,1.73150982030695));
#6141=CARTESIAN_POINT('Ctrl Pts',(3.57485487654503,-0.451266678061753,1.74498214748221));
#6142=CARTESIAN_POINT('Ctrl Pts',(3.57094683261233,-0.517839578446989,1.76201022850709));
#6143=CARTESIAN_POINT('Ctrl Pts',(3.56703878867963,-0.583377636205339,1.78251202330899));
#6144=CARTESIAN_POINT('Ctrl Pts',(3.56313318771024,-0.648874725368399,1.80300100220267));
#6145=CARTESIAN_POINT('Ctrl Pts',(3.55922758674084,-0.713337786867189,1.82695924084957));
#6146=CARTESIAN_POINT('Ctrl Pts',(3.55532198577145,-0.776379002835167,1.85425430534159));
#6147=CARTESIAN_POINT('Ctrl Pts',(3.55141748750173,-0.839402419870669,1.88154166339898));
#6148=CARTESIAN_POINT('Ctrl Pts',(3.547512989232,-0.901004337255898,1.91216378171569));
#6149=CARTESIAN_POINT('Ctrl Pts',(3.54360849096228,-0.960816693256813,1.94594000754769));
#6150=CARTESIAN_POINT('Ctrl Pts',(3.53970375676551,-1.0206326633847,1.97971827428858));
#6151=CARTESIAN_POINT('Ctrl Pts',(3.53579902256873,-1.0786584305169,2.01665078287648));
#6152=CARTESIAN_POINT('Ctrl Pts',(3.53189428837196,-1.13455192769951,2.05651171856492));
#6153=CARTESIAN_POINT('Ctrl Pts',(3.52798539964158,-1.19050489408061,2.09641506523167));
#6154=CARTESIAN_POINT('Ctrl Pts',(3.52407651091119,-1.24432066185106,2.13925277096336));
#6155=CARTESIAN_POINT('Ctrl Pts',(3.5201676221808,-1.29568831620729,2.18475719703583));
#6156=CARTESIAN_POINT('Ctrl Pts',(3.51625639055101,-1.34708675917252,2.23028889743101));
#6157=CARTESIAN_POINT('Ctrl Pts',(3.51234515892122,-1.3960338180056,2.27849015414664));
#6158=CARTESIAN_POINT('Ctrl Pts',(3.50843392729142,-1.44225572602493,2.32905671916633));
#6159=CARTESIAN_POINT('Ctrl Pts',(3.50451596368841,-1.48855719073542,2.37971031885788));
#6160=CARTESIAN_POINT('Ctrl Pts',(3.50059800008541,-1.53212383128964,2.43273697234076));
#6161=CARTESIAN_POINT('Ctrl Pts',(3.4966800364824,-1.57272296308931,2.48780036629318));
#6162=CARTESIAN_POINT('Ctrl Pts',(3.49486297899153,-1.59155186606905,2.51333744692786));
#6163=CARTESIAN_POINT('Ctrl Pts',(3.49304592150067,-1.60974311680241,2.5393122153768));
#6164=CARTESIAN_POINT('Ctrl Pts',(3.4912288640098,-1.62727683669187,2.56568928813259));
#6165=CARTESIAN_POINT('Ctrl Pts',(3.48724042291459,-1.66576335091086,2.62358696141989));
#6166=CARTESIAN_POINT('Ctrl Pts',(3.48325198181939,-1.70122719124068,2.68364762603425));
#6167=CARTESIAN_POINT('Ctrl Pts',(3.47926354072418,-1.73342304991812,2.7455294395725));
#6168=CARTESIAN_POINT('Ctrl Pts',(3.47528172814961,-1.76556540124562,2.80730840970205));
#6169=CARTESIAN_POINT('Ctrl Pts',(3.47129991557503,-1.79445034260521,2.87090210568594));
#6170=CARTESIAN_POINT('Ctrl Pts',(3.46731810300046,-1.81987604930015,2.93594020750271));
#6171=CARTESIAN_POINT('Ctrl Pts',(3.46334277468661,-1.84526035100472,3.00087239674792));
#6172=CARTESIAN_POINT('Ctrl Pts',(3.45936744637276,-1.8671964512743,3.06724388003304));
#6173=CARTESIAN_POINT('Ctrl Pts',(3.45539211805891,-1.8855294599695,3.13466193022225));
#6174=CARTESIAN_POINT('Ctrl Pts',(3.45142059332048,-1.90384492772825,3.20201547513826));
#6175=CARTESIAN_POINT('Ctrl Pts',(3.44744906858206,-1.91856402806981,3.27041314777312));
#6176=CARTESIAN_POINT('Ctrl Pts',(3.44347754384363,-1.92958115826756,3.33944552177032));
#6177=CARTESIAN_POINT('Ctrl Pts',(3.4395087631665,-1.94059067635599,3.40843019895639));
#6178=CARTESIAN_POINT('Ctrl Pts',(3.43553998248937,-1.94790323385196,3.47804824402521));
#6179=CARTESIAN_POINT('Ctrl Pts',(3.43157120181223,-1.95146428769482,3.54787997762178));
#6180=CARTESIAN_POINT('Ctrl Pts',(3.4296706985829,-1.95316954552557,3.581319828802));
#6181=CARTESIAN_POINT('Ctrl Pts',(3.42777019535356,-1.9540153051049,3.61480856012914));
#6182=CARTESIAN_POINT('Ctrl Pts',(3.42586969212423,-1.95399979033479,3.64829965974897));
#6183=CARTESIAN_POINT('Ctrl Pts',(3.32413030787577,-1.95399983251336,3.64820350335859));
#6184=CARTESIAN_POINT('Ctrl Pts',(3.32811085978269,-1.95402888143147,3.57804389856121));
#6185=CARTESIAN_POINT('Ctrl Pts',(3.33209141168961,-1.95027489940237,3.50790303752685));
#6186=CARTESIAN_POINT('Ctrl Pts',(3.33607196359653,-1.94277019996061,3.43820567760661));
#6187=CARTESIAN_POINT('Ctrl Pts',(3.34005484693765,-1.93526110496934,3.36846749550572));
#6188=CARTESIAN_POINT('Ctrl Pts',(3.34403773027878,-1.92399697641733,3.29917379235574));
#6189=CARTESIAN_POINT('Ctrl Pts',(3.34802061361991,-1.90906168828384,3.23074177079247));
#6190=CARTESIAN_POINT('Ctrl Pts',(3.35201014553545,-1.89410146887164,3.16219551656176));
#6191=CARTESIAN_POINT('Ctrl Pts',(3.355999677451,-1.87545795844438,3.09451426921831));
#6192=CARTESIAN_POINT('Ctrl Pts',(3.35998920936655,-1.85326551711363,3.02810219231269));
#6193=CARTESIAN_POINT('Ctrl Pts',(3.36398253485343,-1.83105197340516,2.96162696540429));
#6194=CARTESIAN_POINT('Ctrl Pts',(3.36797586034032,-1.80528295013365,2.89642374333976));
#6195=CARTESIAN_POINT('Ctrl Pts',(3.37196918582721,-1.77614075125022,2.83287618626172));
#6196=CARTESIAN_POINT('Ctrl Pts',(3.37597065791847,-1.74693910067274,2.76919898866013));
#6197=CARTESIAN_POINT('Ctrl Pts',(3.37997213000974,-1.71435075203511,2.70718460986591));
#6198=CARTESIAN_POINT('Ctrl Pts',(3.38397360210101,-1.67860342342431,2.64719121550563));
#6199=CARTESIAN_POINT('Ctrl Pts',(3.38538917625688,-1.66595732884491,2.6259677515797));
#6200=CARTESIAN_POINT('Ctrl Pts',(3.38680475041276,-1.65291627738981,2.60499692950161));
#6201=CARTESIAN_POINT('Ctrl Pts',(3.38822032456863,-1.63949157496413,2.58429363787237));
#6202=CARTESIAN_POINT('Ctrl Pts',(3.39213901376762,-1.60232839550313,2.52698136994608));
#6203=CARTESIAN_POINT('Ctrl Pts',(3.3960577029666,-1.56208293473802,2.47150688257569));
#6204=CARTESIAN_POINT('Ctrl Pts',(3.39997639216559,-1.51896302007941,2.4182210290853));
#6205=CARTESIAN_POINT('Ctrl Pts',(3.40388919137145,-1.47590791688919,2.36501526699669));
#6206=CARTESIAN_POINT('Ctrl Pts',(3.4078019905773,-1.42998724131859,2.31399198913342));
#6207=CARTESIAN_POINT('Ctrl Pts',(3.41171478978316,-1.38145230970952,2.26547351685494));
#6208=CARTESIAN_POINT('Ctrl Pts',(3.41562299901092,-1.33297431285769,2.21701196002581));
#6209=CARTESIAN_POINT('Ctrl Pts',(3.41953120823868,-1.28188849665403,2.17104971919554));
#6210=CARTESIAN_POINT('Ctrl Pts',(3.42343941746644,-1.22848549620142,2.12787500950003));
#6211=CARTESIAN_POINT('Ctrl Pts',(3.42734518432627,-1.17511586903248,2.08472728109437));
#6212=CARTESIAN_POINT('Ctrl Pts',(3.43125095118611,-1.1194323117201,2.04436393660728));
#6213=CARTESIAN_POINT('Ctrl Pts',(3.43515671804595,-1.06176009971729,2.0070342972701));
#6214=CARTESIAN_POINT('Ctrl Pts',(3.4390613825441,-1.0041041650908,1.96971519383168));
#6215=CARTESIAN_POINT('Ctrl Pts',(3.44296604704225,-0.944461102619715,1.93542836280052));
#6216=CARTESIAN_POINT('Ctrl Pts',(3.4468707115404,-0.88318536029021,1.90437994758444));
#6217=CARTESIAN_POINT('Ctrl Pts',(3.45077561204667,-0.821905914294886,1.8733296557211));
#6218=CARTESIAN_POINT('Ctrl Pts',(3.45468051255293,-0.75899403229621,1.84551838823046));
#6219=CARTESIAN_POINT('Ctrl Pts',(3.45858541305919,-0.694827332237743,1.82110561424807));
#6220=CARTESIAN_POINT('Ctrl Pts',(3.46249446707374,-0.630592380268807,1.7966668732382));
#6221=CARTESIAN_POINT('Ctrl Pts',(3.46640352108827,-0.565100407054626,1.7756340149785));
#6222=CARTESIAN_POINT('Ctrl Pts',(3.47031257510282,-0.49874656330373,1.75811739342356));
#6223=CARTESIAN_POINT('Ctrl Pts',(3.47422397167028,-0.432352956124042,1.74059027479876));
#6224=CARTESIAN_POINT('Ctrl Pts',(3.47813536823775,-0.365096931932403,1.72658368679383));
#6225=CARTESIAN_POINT('Ctrl Pts',(3.48204676480522,-0.297383510812253,1.71615676994196));
#6226=CARTESIAN_POINT('Ctrl Pts',(3.48596489107774,-0.229553586201834,1.70571191318709));
#6227=CARTESIAN_POINT('Ctrl Pts',(3.48988301735025,-0.161265182991503,1.69885906877368));
#6228=CARTESIAN_POINT('Ctrl Pts',(3.49380114362277,-0.0929272280146145,
1.69560540942184));
#6229=CARTESIAN_POINT('Ctrl Pts',(3.49561671746175,-0.061260917478458,1.69409773499042));
#6230=CARTESIAN_POINT('Ctrl Pts',(3.49743229130073,-0.0295839467283565,
1.69336213986674));
#6231=CARTESIAN_POINT('Ctrl Pts',(3.49924786513971,0.00206331676382339,
1.69339555765881));
#6232=CARTESIAN_POINT('Ctrl Pts',(3.50316643928061,0.0703679737754331,1.69346768366824));
#6233=CARTESIAN_POINT('Ctrl Pts',(3.50708501342151,0.138803851921841,1.69712578460811));
#6234=CARTESIAN_POINT('Ctrl Pts',(3.51100358756241,0.206963501706501,1.70438594824043));
#6235=CARTESIAN_POINT('Ctrl Pts',(3.51491627231299,0.275020711479269,1.71163520026668));
#6236=CARTESIAN_POINT('Ctrl Pts',(3.51882895706357,0.342802031772585,1.72247571894332));
#6237=CARTESIAN_POINT('Ctrl Pts',(3.52274164181415,0.409900345716121,1.73687158001956));
#6238=CARTESIAN_POINT('Ctrl Pts',(3.52664973806483,0.476919971846337,1.75125055872182));
#6239=CARTESIAN_POINT('Ctrl Pts',(3.53055783431551,0.543257703856662,1.76917649652727));
#6240=CARTESIAN_POINT('Ctrl Pts',(3.53446593056618,0.608513703120316,1.7905619305695));
#6241=CARTESIAN_POINT('Ctrl Pts',(3.538371585438,0.673728937109304,1.8119340051796));
#6242=CARTESIAN_POINT('Ctrl Pts',(3.54227724030981,0.737863312606935,1.83676113616042));
#6243=CARTESIAN_POINT('Ctrl Pts',(3.54618289518163,0.800530830918063,1.86490564959534));
#6244=CARTESIAN_POINT('Ctrl Pts',(3.55008744885813,0.863180680187841,1.89304222771409));
#6245=CARTESIAN_POINT('Ctrl Pts',(3.55399200253463,0.92436404494093,1.92449413008874));
#6246=CARTESIAN_POINT('Ctrl Pts',(3.55789655621114,0.983715333682244,1.95907573585257));
#6247=CARTESIAN_POINT('Ctrl Pts',(3.5618013472406,1.04307023031451,1.99365944378916));
#6248=CARTESIAN_POINT('Ctrl Pts',(3.56570613827006,1.10059240624667,2.03137298304466));
#6249=CARTESIAN_POINT('Ctrl Pts',(3.56961092929951,1.1559428736939,2.07198592674415));
#6250=CARTESIAN_POINT('Ctrl Pts',(3.57351987663855,1.2113522568875,2.11264209938101));
#6251=CARTESIAN_POINT('Ctrl Pts',(3.57742882397759,1.26458492120601,2.15620354395477));
#6252=CARTESIAN_POINT('Ctrl Pts',(3.58133777131662,1.31533359401786,2.20239843491629));
#6253=CARTESIAN_POINT('Ctrl Pts',(3.58524906265562,1.36611269826724,2.24862102664042));
#6254=CARTESIAN_POINT('Ctrl Pts',(3.58916035399461,1.41440450085385,2.29747985777418));
#6255=CARTESIAN_POINT('Ctrl Pts',(3.5930716453336,1.4599393691669,2.34866699942962));
#6256=CARTESIAN_POINT('Ctrl Pts',(3.59698966972396,1.50555262300048,2.39994225665214));
#6257=CARTESIAN_POINT('Ctrl Pts',(3.60090769411433,1.54839916383622,2.45355343977741));
#6258=CARTESIAN_POINT('Ctrl Pts',(3.60482571850469,1.58825087105815,2.50916111321865));
#6259=CARTESIAN_POINT('Ctrl Pts',(3.60664228090672,1.60672781397207,2.53494319081015));
#6260=CARTESIAN_POINT('Ctrl Pts',(3.60845884330875,1.6245616033113,2.56115406024023));
#6261=CARTESIAN_POINT('Ctrl Pts',(3.61027540571078,1.64173285670969,2.58775810273207));
#6262=CARTESIAN_POINT('Ctrl Pts',(3.61419379700105,1.67877187594958,2.64514399174387));
#6263=CARTESIAN_POINT('Ctrl Pts',(3.61811218829132,1.71287172113914,2.70458778327021));
#6264=CARTESIAN_POINT('Ctrl Pts',(3.62203057958159,1.74379755342962,2.76575616792886));
#6265=CARTESIAN_POINT('Ctrl Pts',(3.62594307766091,1.77467687365945,2.82683255611058));
#6266=CARTESIAN_POINT('Ctrl Pts',(3.62985557574024,1.80239143499202,2.88962795431));
#6267=CARTESIAN_POINT('Ctrl Pts',(3.63376807381956,1.82675024602289,2.95378107549555));
#6268=CARTESIAN_POINT('Ctrl Pts',(3.63767597865819,1.8510804600091,3.01785888144223));
#6269=CARTESIAN_POINT('Ctrl Pts',(3.64158388349681,1.87206257414127,3.08329078713651));
#6270=CARTESIAN_POINT('Ctrl Pts',(3.64549178833543,1.88955282088803,3.14969361729596));
#6271=CARTESIAN_POINT('Ctrl Pts',(3.6493972489622,1.90703212830279,3.21605491558825));
#6272=CARTESIAN_POINT('Ctrl Pts',(3.65330270958897,1.92102377574857,3.2833854591959));
#6273=CARTESIAN_POINT('Ctrl Pts',(3.65720817021574,1.93143366978041,3.35128641496791));
#6274=CARTESIAN_POINT('Ctrl Pts',(3.66111252710871,1.94184062184128,3.41916818104976));
#6275=CARTESIAN_POINT('Ctrl Pts',(3.66501688400169,1.94866775551528,3.48761955338122));
#6276=CARTESIAN_POINT('Ctrl Pts',(3.66892124089467,1.9518723184559,3.55623278529371));
#6277=CARTESIAN_POINT('Ctrl Pts',(3.67282583289382,1.95507707436365,3.62485014884565));
#6278=CARTESIAN_POINT('Ctrl Pts',(3.67673042489298,1.95465880608775,3.69362889995242));
#6279=CARTESIAN_POINT('Ctrl Pts',(3.68063501689214,1.9506268316063,3.76215928788278));
#6280=CARTESIAN_POINT('Ctrl Pts',(3.68454376315515,1.94659056733328,3.83076258824888));
#6281=CARTESIAN_POINT('Ctrl Pts',(3.68845250941816,1.9389329528984,3.89911650621338));
#6282=CARTESIAN_POINT('Ctrl Pts',(3.69236125568117,1.92771529253682,3.9668154302129));
#6283=CARTESIAN_POINT('Ctrl Pts',(3.69627234448219,1.9164909093557,4.03455492663443));
#6284=CARTESIAN_POINT('Ctrl Pts',(3.70018343328321,1.9017023399558,4.10163816753919));
#6285=CARTESIAN_POINT('Ctrl Pts',(3.70409452208423,1.88346164729882,4.16767153212047));
#6286=CARTESIAN_POINT('Ctrl Pts',(3.70801234379548,1.86518955342533,4.23381857264685));
#6287=CARTESIAN_POINT('Ctrl Pts',(3.71193016550673,1.84345363127498,4.29891166351238));
#6288=CARTESIAN_POINT('Ctrl Pts',(3.71584798721798,1.81841494640197,4.36257492292585));
#6289=CARTESIAN_POINT('Ctrl Pts',(3.71766630690595,1.80679411803847,4.39212199436581));
#6290=CARTESIAN_POINT('Ctrl Pts',(3.71948462659391,1.79446252923629,4.42136139692663));
#6291=CARTESIAN_POINT('Ctrl Pts',(3.72130294628187,1.78143961641532,4.45025740370065));
#6292=CARTESIAN_POINT('Ctrl Pts',(3.72522147186894,1.75337490510792,4.51252903979293));
#6293=CARTESIAN_POINT('Ctrl Pts',(3.72913999745602,1.72198563863023,4.57345050024927));
#6294=CARTESIAN_POINT('Ctrl Pts',(3.73305852304309,1.6874241453808,4.63264355028591));
#6295=CARTESIAN_POINT('Ctrl Pts',(3.73697115741272,1.65291461281587,4.69174760788883));
#6296=CARTESIAN_POINT('Ctrl Pts',(3.74088379178235,1.61524256473294,4.74912799103301));
#6297=CARTESIAN_POINT('Ctrl Pts',(3.74479642615199,1.57460763543134,4.804428086828));
#6298=CARTESIAN_POINT('Ctrl Pts',(3.74870446955744,1.5340203858993,4.85966329520053));
#6299=CARTESIAN_POINT('Ctrl Pts',(3.75261251296288,1.49047744950318,4.91282266960529));
#6300=CARTESIAN_POINT('Ctrl Pts',(3.75652055636833,1.44422248756346,4.9635773607483));
#6301=CARTESIAN_POINT('Ctrl Pts',(3.76042615689386,1.39799643915049,5.01430032562759));
#6302=CARTESIAN_POINT('Ctrl Pts',(3.7643317574194,1.34906205859251,5.06262122638954));
#6303=CARTESIAN_POINT('Ctrl Pts',(3.76823735794493,1.29770313383148,5.10824441829378));
#6304=CARTESIAN_POINT('Ctrl Pts',(3.77214185585457,1.24635870854784,5.15385473001327));
#6305=CARTESIAN_POINT('Ctrl Pts',(3.77604635376421,1.19259146538888,5.196768518388));
#6306=CARTESIAN_POINT('Ctrl Pts',(3.77995085167385,1.13672056180759,5.23672840561858));
#6307=CARTESIAN_POINT('Ctrl Pts',(3.78385558559481,1.08084628105307,5.27669070826492));
#6308=CARTESIAN_POINT('Ctrl Pts',(3.78776031951578,1.0228684889009,5.31369847130271));
#6309=CARTESIAN_POINT('Ctrl Pts',(3.79166505343674,0.963136307333333,5.34753694863554));
#6310=CARTESIAN_POINT('Ctrl Pts',(3.79557394202005,0.90334057033524,5.3814114303288));
#6311=CARTESIAN_POINT('Ctrl Pts',(3.79948283060335,0.841787147330355,5.41210965379722));
#6312=CARTESIAN_POINT('Ctrl Pts',(3.80339171918666,0.778849921474264,5.43946277050327));
#6313=CARTESIAN_POINT('Ctrl Pts',(3.80730295074269,0.715874971288073,5.46683228256184));
#6314=CARTESIAN_POINT('Ctrl Pts',(3.81121418229871,0.651515028264088,5.49085252547173));
#6315=CARTESIAN_POINT('Ctrl Pts',(3.81512541385474,0.586161478091734,5.51140378199486));
#6316=CARTESIAN_POINT('Ctrl Pts',(3.81904337749726,0.520695440139974,5.53199041173343));
#6317=CARTESIAN_POINT('Ctrl Pts',(3.82296134113978,0.454232857736643,5.54909601583925));
#6318=CARTESIAN_POINT('Ctrl Pts',(3.8268793047823,0.38717683906159,5.56265165605116));
#6319=CARTESIAN_POINT('Ctrl Pts',(3.82869636547251,0.356077812451394,5.56893844766209));
#6320=CARTESIAN_POINT('Ctrl Pts',(3.83051342616273,0.324851235324714,5.57446241188905));
#6321=CARTESIAN_POINT('Ctrl Pts',(3.83233048685294,0.293537575865702,5.57922046757959));
#6322=CARTESIAN_POINT('Ctrl Pts',(3.83624898600517,0.226009535275453,5.58948123503227));
#6323=CARTESIAN_POINT('Ctrl Pts',(3.84016748515741,0.157809303592916,5.59621731169598));
#6324=CARTESIAN_POINT('Ctrl Pts',(3.84408598430965,0.089337189589276,5.59935114468739));
#6325=CARTESIAN_POINT('Ctrl Pts',(3.84799859215053,0.0209680207508368,5.60248026608256));
#6326=CARTESIAN_POINT('Ctrl Pts',(3.85191119999142,-0.0476717318334287,
5.60201787010987));
#6327=CARTESIAN_POINT('Ctrl Pts',(3.8558238078323,-0.116174217615536,5.59793786722721));
#6328=CARTESIAN_POINT('Ctrl Pts',(3.85973182470374,-0.184596324061974,5.5938626517317));
#6329=CARTESIAN_POINT('Ctrl Pts',(3.86363984157518,-0.252880995006901,5.5861782887664));
#6330=CARTESIAN_POINT('Ctrl Pts',(3.86754785844663,-0.320619775905069,5.57491073521875));
#6331=CARTESIAN_POINT('Ctrl Pts',(3.8714534324511,-0.388316213887179,5.56365022491971));
#6332=CARTESIAN_POINT('Ctrl Pts',(3.87535900645557,-0.455466954708045,5.54881104769211));
#6333=CARTESIAN_POINT('Ctrl Pts',(3.87926458046004,-0.521669626871883,5.53047088744464));
#6334=CARTESIAN_POINT('Ctrl Pts',(3.88316905190291,-0.587853609715083,5.51213590470926));
#6335=CARTESIAN_POINT('Ctrl Pts',(3.88707352334577,-0.653089581536215,5.49030203224688));
#6336=CARTESIAN_POINT('Ctrl Pts',(3.89097799478863,-0.716988088420454,5.46509743661043));
#6337=CARTESIAN_POINT('Ctrl Pts',(3.89488270233848,-0.780890459306206,5.43989131682888));
#6338=CARTESIAN_POINT('Ctrl Pts',(3.89878740988832,-0.843454748171191,5.41131425203775));
#6339=CARTESIAN_POINT('Ctrl Pts',(3.90269211743816,-0.904311019378601,5.3795427241299));
#6340=CARTESIAN_POINT('Ctrl Pts',(3.90660097997775,-0.965232047595143,5.34773738821702));
#6341=CARTESIAN_POINT('Ctrl Pts',(3.91050984251733,-1.02444099427484,5.31273103349862));
#6342=CARTESIAN_POINT('Ctrl Pts',(3.91441870505691,-1.08159301051947,5.27474586229668));
#6343=CARTESIAN_POINT('Ctrl Pts',(3.91832991071858,-1.13877928587395,5.2367379213267));
#6344=CARTESIAN_POINT('Ctrl Pts',(3.92224111638024,-1.19390578221183,5.19574790362305));
#6345=CARTESIAN_POINT('Ctrl Pts',(3.9261523220419,-1.24665939534115,5.15203939384194));
#6346=CARTESIAN_POINT('Ctrl Pts',(3.93007026029319,-1.29950381638485,5.10825564601781));
#6347=CARTESIAN_POINT('Ctrl Pts',(3.93398819854449,-1.34996684078181,5.06174439981745));
#6348=CARTESIAN_POINT('Ctrl Pts',(3.93790613679579,-1.39777163204783,5.01280666415819));
#6349=CARTESIAN_POINT('Ctrl Pts',(3.93972343367186,-1.41994541127995,4.99010737988375));
#6350=CARTESIAN_POINT('Ctrl Pts',(3.94154073054794,-1.44154784196988,4.9668865155006));
#6351=CARTESIAN_POINT('Ctrl Pts',(3.94335802742402,-1.46255434627852,4.94317638827728));
#6352=CARTESIAN_POINT('Ctrl Pts',(3.94723899460202,-1.50741523544837,4.89254171941756));
#6353=CARTESIAN_POINT('Ctrl Pts',(3.95111996178003,-1.54974101147079,4.83946434287412));
#6354=CARTESIAN_POINT('Ctrl Pts',(3.95500092895803,-1.58925110793402,4.78423083114816));
#6355=CARTESIAN_POINT('Ctrl Pts',(3.95887649205015,-1.62870618822607,4.72907422979721));
#6356=CARTESIAN_POINT('Ctrl Pts',(3.96275205514227,-1.66535307107133,4.67176784819088));
#6357=CARTESIAN_POINT('Ctrl Pts',(3.96662761823439,-1.69894984269427,4.61263300461006));
#6358=CARTESIAN_POINT('Ctrl Pts',(3.97049917545996,-1.73251188796124,4.55355928409343));
#6359=CARTESIAN_POINT('Ctrl Pts',(3.97437073268553,-1.76302982718918,4.49266128331292));
#6360=CARTESIAN_POINT('Ctrl Pts',(3.97824228991111,-1.79030481181491,4.43028953200083));
#6361=CARTESIAN_POINT('Ctrl Pts',(3.98211211898432,-1.81756762166798,4.36794562165374));
#6362=CARTESIAN_POINT('Ctrl Pts',(3.98598194805753,-1.84159013640098,4.30412971952778));
#6363=CARTESIAN_POINT('Ctrl Pts',(3.98985177713074,-1.86222007239048,4.23921572676147));
#6364=CARTESIAN_POINT('Ctrl Pts',(3.99372037176401,-1.88284342761977,4.17432244096296));
#6365=CARTESIAN_POINT('Ctrl Pts',(3.99758896639727,-1.90007620415422,4.10833223942717));
#6366=CARTESIAN_POINT('Ctrl Pts',(4.00145756103053,-1.91381554134512,4.04163560478018));
#6367=CARTESIAN_POINT('Ctrl Pts',(4.00532869478215,-1.92756389623018,3.97489519437857));
#6368=CARTESIAN_POINT('Ctrl Pts',(4.00919982853377,-1.93781412805715,3.90744791692283));
#6369=CARTESIAN_POINT('Ctrl Pts',(4.01307096228539,-1.94451449325918,3.83969471660667));
#6370=CARTESIAN_POINT('Ctrl Pts',(4.01675741081552,-1.95089519540876,3.77517390649201));
#6371=CARTESIAN_POINT('Ctrl Pts',(4.02044385934564,-1.95405702262766,3.71037610742807));
#6372=CARTESIAN_POINT('Ctrl Pts',(4.02413030787577,-1.95399922086809,3.64564951931539));
#6373=CARTESIAN_POINT('Origin',(0.,0.,3.64739446828387));
#6374=CARTESIAN_POINT('',(4.82586969212423,-1.95430222507481,3.64764326884653));
#6375=CARTESIAN_POINT('',(4.72413035081973,-1.95427619993066,3.64777710414201));
#6376=CARTESIAN_POINT('',(0.,-1.954,3.64739446828387));
#6377=CARTESIAN_POINT('Ctrl Pts',(4.82586969212423,-1.95715633972901,3.64764363220145));
#6378=CARTESIAN_POINT('Ctrl Pts',(4.8250995783704,-1.95718052860821,3.66109012482263));
#6379=CARTESIAN_POINT('Ctrl Pts',(4.78732028442627,-1.95096916696084,4.32070869776121));
#6380=CARTESIAN_POINT('Ctrl Pts',(4.71253181029161,-1.21359828804363,5.61146159126675));
#6381=CARTESIAN_POINT('Ctrl Pts',(4.60150426972061,0.989869636257431,5.73318883630089));
#6382=CARTESIAN_POINT('Ctrl Pts',(4.49047672914949,2.28894570144034,3.94923537617159));
#6383=CARTESIAN_POINT('Ctrl Pts',(4.37944918857844,1.49673214248603,1.88950560619213));
#6384=CARTESIAN_POINT('Ctrl Pts',(4.26842164800734,-0.662966995866537,1.43586675992707));
#6385=CARTESIAN_POINT('Ctrl Pts',(4.18389531480082,-1.8460276791096,2.62877633203429));
#6386=CARTESIAN_POINT('Ctrl Pts',(4.13637816178465,-1.95459509422112,3.46119040754887));
#6387=CARTESIAN_POINT('Ctrl Pts',(4.12587018895884,-1.95303263999471,3.6456699100979));
#6388=CARTESIAN_POINT('Ctrl Pts',(4.02413030792419,-1.95399922086733,3.64564951846532));
#6389=CARTESIAN_POINT('Ctrl Pts',(4.02917285126934,-1.95392015614755,3.55711264524746));
#6390=CARTESIAN_POINT('Ctrl Pts',(4.03421539461449,-1.94781926961924,3.46884243996873));
#6391=CARTESIAN_POINT('Ctrl Pts',(4.03925793795964,-1.93583046129939,3.38154408723206));
#6392=CARTESIAN_POINT('Ctrl Pts',(4.0443004813048,-1.92384165297954,3.29424573449538));
#6393=CARTESIAN_POINT('Ctrl Pts',(4.04934302464995,-1.90596512136721,3.20791897386854));
#6394=CARTESIAN_POINT('Ctrl Pts',(4.05438556799511,-1.88238740014386,3.12324403588909));
#6395=CARTESIAN_POINT('Ctrl Pts',(4.0583040649868,-1.86406544961994,3.05744420690733));
#6396=CARTESIAN_POINT('Ctrl Pts',(4.06222256197849,-1.84225301252198,2.99247609015028));
#6397=CARTESIAN_POINT('Ctrl Pts',(4.06614105897018,-1.81704344396077,2.92873660618314));
#6398=CARTESIAN_POINT('Ctrl Pts',(4.07005366446439,-1.79187177822557,2.86509295513616));
#6399=CARTESIAN_POINT('Ctrl Pts',(4.0739662699586,-1.76331329734956,2.80267472432131));
#6400=CARTESIAN_POINT('Ctrl Pts',(4.07787887545281,-1.73151138885174,2.74186461771199));
#6401=CARTESIAN_POINT('Ctrl Pts',(4.08178688971242,-1.69974679820328,2.68112586853074));
#6402=CARTESIAN_POINT('Ctrl Pts',(4.08569490397203,-1.66474656556231,2.62199192953893));
#6403=CARTESIAN_POINT('Ctrl Pts',(4.08960291823164,-1.62670179878594,2.56482472095736));
#6404=CARTESIAN_POINT('Ctrl Pts',(4.09350848946089,-1.5886808150652,2.50769324950909));
#6405=CARTESIAN_POINT('Ctrl Pts',(4.09741406069013,-1.54761934451823,2.45252647804732));
#6406=CARTESIAN_POINT('Ctrl Pts',(4.10131963191938,-1.503753182883,2.39965957457879));
#6407=CARTESIAN_POINT('Ctrl Pts',(4.10522410042749,-1.45989940666873,2.34680759785172));
#6408=CARTESIAN_POINT('Ctrl Pts',(4.10912856893559,-1.41324282530704,2.2962545782837));
#6409=CARTESIAN_POINT('Ctrl Pts',(4.1130330374437,-1.36405998580495,2.24830320781306));
#6410=CARTESIAN_POINT('Ctrl Pts',(4.11693774190294,-1.31487417413215,2.20034893959068));
#6411=CARTESIAN_POINT('Ctrl Pts',(4.12084244636218,-1.2631621551327,2.15499697405001));
#6412=CARTESIAN_POINT('Ctrl Pts',(4.12474715082143,-1.20923654449766,2.11251239481654));
#6413=CARTESIAN_POINT('Ctrl Pts',(4.12865601005464,-1.15525355468686,2.06998261015824));
#6414=CARTESIAN_POINT('Ctrl Pts',(4.13256486928786,-1.09905265975336,2.03032660554053));
#6415=CARTESIAN_POINT('Ctrl Pts',(4.13647372852107,-1.04097789456905,1.99376784083178));
#6416=CARTESIAN_POINT('Ctrl Pts',(4.14038493074819,-0.982868319018695,1.957187162578));
#6417=CARTESIAN_POINT('Ctrl Pts',(4.1442961329753,-0.922883067278713,1.92370765872149));
#6418=CARTESIAN_POINT('Ctrl Pts',(4.14820733520242,-0.861390907329552,1.89350687075375));
#6419=CARTESIAN_POINT('Ctrl Pts',(4.15212526985654,-0.799792899752562,1.86325409759363));
#6420=CARTESIAN_POINT('Ctrl Pts',(4.15604320451065,-0.736683259058302,1.8362914971923));
#6421=CARTESIAN_POINT('Ctrl Pts',(4.15996113916476,-0.672450022015205,1.81274818959913));
#6422=CARTESIAN_POINT('Ctrl Pts',(4.16177846229857,-0.642655612985202,1.801827691604));
#6423=CARTESIAN_POINT('Ctrl Pts',(4.16359578543237,-0.612619657991507,1.79164216046196));
#6424=CARTESIAN_POINT('Ctrl Pts',(4.16541310856617,-0.58238171102534,1.78220076717313));
#6425=CARTESIAN_POINT('Ctrl Pts',(4.16933160051186,-0.51718298580306,1.7618433398834));
#6426=CARTESIAN_POINT('Ctrl Pts',(4.17325009245754,-0.450786632722358,1.74486834658914));
#6427=CARTESIAN_POINT('Ctrl Pts',(4.17716858440322,-0.383576620845942,1.73141300283583));
#6428=CARTESIAN_POINT('Ctrl Pts',(4.1810811848136,-0.31646766064036,1.71797788947573));
#6429=CARTESIAN_POINT('Ctrl Pts',(4.18499378522397,-0.248547947918793,1.7080520188436));
#6430=CARTESIAN_POINT('Ctrl Pts',(4.18890638563434,-0.18021669174885,1.70172287625836));
#6431=CARTESIAN_POINT('Ctrl Pts',(4.19281439477959,-0.111965619313588,1.69540116064458));
#6432=CARTESIAN_POINT('Ctrl Pts',(4.19672240392484,-0.0433044499019896,
1.69266783597897));
#6433=CARTESIAN_POINT('Ctrl Pts',(4.20063041307009,0.0253591372019198,1.69355903146726));
#6434=CARTESIAN_POINT('Ctrl Pts',(4.20453597916911,0.0939798000670118,1.6944496698351));
#6435=CARTESIAN_POINT('Ctrl Pts',(4.20844154526813,0.162602386999144,1.69896032725903));
#6436=CARTESIAN_POINT('Ctrl Pts',(4.21234711136715,0.230817406905028,1.707075081));
#6437=CARTESIAN_POINT('Ctrl Pts',(4.21625157473709,0.299013166431403,1.71518754355589));
#6438=CARTESIAN_POINT('Ctrl Pts',(4.22015603810705,0.36680109928512,1.72690202420201));
#6439=CARTESIAN_POINT('Ctrl Pts',(4.224060501477,0.433776846712702,1.7421507444375));
#6440=CARTESIAN_POINT('Ctrl Pts',(4.22796520079809,0.500756641560616,1.75740038617044));
#6441=CARTESIAN_POINT('Ctrl Pts',(4.23186990011919,0.566923674618865,1.77618457983965));
#6442=CARTESIAN_POINT('Ctrl Pts',(4.23577459944029,0.631885572091681,1.79838483505251));
#6443=CARTESIAN_POINT('Ctrl Pts',(4.2396834535708,0.696916592506178,1.82060871252713));
#6444=CARTESIAN_POINT('Ctrl Pts',(4.24359230770132,0.760739452005175,1.8462557462092));
#6445=CARTESIAN_POINT('Ctrl Pts',(4.24750116183184,0.822979658705006,1.87515845652985));
#6446=CARTESIAN_POINT('Ctrl Pts',(4.25141235896911,0.885257172815203,1.90407849142784));
#6447=CARTESIAN_POINT('Ctrl Pts',(4.25532355610639,0.945949711592333,1.93625785640229));
#6448=CARTESIAN_POINT('Ctrl Pts',(4.25923475324367,1.00470790265021,1.9714833637344));
#6449=CARTESIAN_POINT('Ctrl Pts',(4.26315268288125,1.06356723653613,2.00676950614337));
#6450=CARTESIAN_POINT('Ctrl Pts',(4.26707061251884,1.12048516969906,2.04511198123528));
#6451=CARTESIAN_POINT('Ctrl Pts',(4.27098854215643,1.17514251896321,2.08625512148462));
#6452=CARTESIAN_POINT('Ctrl Pts',(4.27280591115004,1.20049585121115,2.10533975911356));
#6453=CARTESIAN_POINT('Ctrl Pts',(4.27462328014365,1.22536326940056,2.12502645043353));
#6454=CARTESIAN_POINT('Ctrl Pts',(4.27644064913727,1.24971558638332,2.14528696442451));
#6455=CARTESIAN_POINT('Ctrl Pts',(4.2803591387095,1.30222242483608,2.18897133071489));
#6456=CARTESIAN_POINT('Ctrl Pts',(4.28427762828174,1.35253983626061,2.23549850288804));
#6457=CARTESIAN_POINT('Ctrl Pts',(4.28819611785398,1.40034404905103,2.28462062633967));
#6458=CARTESIAN_POINT('Ctrl Pts',(4.29210871583145,1.44807638643019,2.33366889285235));
#6459=CARTESIAN_POINT('Ctrl Pts',(4.29602131380893,1.49330268437295,2.3853040176659));
#6460=CARTESIAN_POINT('Ctrl Pts',(4.29993391178641,1.53573264762285,2.43923833804849));
#6461=CARTESIAN_POINT('Ctrl Pts',(4.30384191842259,1.57811282031326,2.49310936778028));
#6462=CARTESIAN_POINT('Ctrl Pts',(4.30774992505877,1.61770287270592,2.54927384999249));
#6463=CARTESIAN_POINT('Ctrl Pts',(4.31165793169496,1.65425102822597,2.60740911472676));
#6464=CARTESIAN_POINT('Ctrl Pts',(4.31556349523904,1.69077633565022,2.66550803617422));
#6465=CARTESIAN_POINT('Ctrl Pts',(4.31946905878312,1.72426325734888,2.72557488075033));
#6466=CARTESIAN_POINT('Ctrl Pts',(4.3233746223272,1.75450273635886,2.78725718382907));
#6467=CARTESIAN_POINT('Ctrl Pts',(4.3272790831002,1.78473367697923,2.84892207035328));
#6468=CARTESIAN_POINT('Ctrl Pts',(4.33118354387319,1.81171877886262,2.91220106849717));
#6469=CARTESIAN_POINT('Ctrl Pts',(4.33508800464619,1.83529531184884,2.97671785596937));
#6470=CARTESIAN_POINT('Ctrl Pts',(4.33899270133211,1.85887326936183,3.04123854163518));
#6471=CARTESIAN_POINT('Ctrl Pts',(4.34289739801803,1.87904208272451,3.10699670233859));
#6472=CARTESIAN_POINT('Ctrl Pts',(4.34680209470395,1.89568811035569,3.17359853303739));
#6473=CARTESIAN_POINT('Ctrl Pts',(4.35071094615929,1.91235185009415,3.24027123102042));
#6474=CARTESIAN_POINT('Ctrl Pts',(4.35461979761464,1.92548520407722,3.30778891251322));
#6475=CARTESIAN_POINT('Ctrl Pts',(4.35852864906998,1.93502537597306,3.37574617666339));
#6476=CARTESIAN_POINT('Ctrl Pts',(4.36243984350534,1.94457126628318,3.4437441746488));
#6477=CARTESIAN_POINT('Ctrl Pts',(4.36635103794069,1.950519645517,3.51218178970461));
#6478=CARTESIAN_POINT('Ctrl Pts',(4.37026223237604,1.95285973907249,3.580649884161));
#6479=CARTESIAN_POINT('Ctrl Pts',(4.37418015929856,1.95520386071968,3.6492358353426));
#6480=CARTESIAN_POINT('Ctrl Pts',(4.37809808622109,1.95392730970642,3.71785187923872));
#6481=CARTESIAN_POINT('Ctrl Pts',(4.38201601314362,1.94907137633538,3.78609115155389));
#6482=CARTESIAN_POINT('Ctrl Pts',(4.38383340533186,1.94681887506375,3.81774501414223));
#6483=CARTESIAN_POINT('Ctrl Pts',(4.3856507975201,1.9437969214201,3.84931791374553));
#6484=CARTESIAN_POINT('Ctrl Pts',(4.38746818970834,1.94001336524288,3.88077000830249));
#6485=CARTESIAN_POINT('Ctrl Pts',(4.39138668198172,1.93185561275431,3.94858409394712));
#6486=CARTESIAN_POINT('Ctrl Pts',(4.39530517425511,1.92012173726112,4.0161040377949));
#6487=CARTESIAN_POINT('Ctrl Pts',(4.39922366652849,1.90484397768049,4.08292336594093));
#6488=CARTESIAN_POINT('Ctrl Pts',(4.40313626725048,1.8895891885945,4.14964222955149));
#6489=CARTESIAN_POINT('Ctrl Pts',(4.40704886797247,1.87080119907181,4.21566209253637));
#6490=CARTESIAN_POINT('Ctrl Pts',(4.41096146869446,1.84856385522711,4.28058296561141));
#6491=CARTESIAN_POINT('Ctrl Pts',(4.41486947812581,1.82635260607386,4.34542765646954));
#6492=CARTESIAN_POINT('Ctrl Pts',(4.41877748755716,1.80070020003049,4.4091754556096));
#6493=CARTESIAN_POINT('Ctrl Pts',(4.42268549698851,1.77174079835075,4.47143969972415));
#6494=CARTESIAN_POINT('Ctrl Pts',(4.42659106335757,1.74279950042006,4.53366501982144));
#6495=CARTESIAN_POINT('Ctrl Pts',(4.43049662972664,1.71055551477644,4.59440817974511));
#6496=CARTESIAN_POINT('Ctrl Pts',(4.4344021960957,1.67519122308988,4.65330220067418));
#6497=CARTESIAN_POINT('Ctrl Pts',(4.43830665971918,1.63983691659182,4.71217959274199));
#6498=CARTESIAN_POINT('Ctrl Pts',(4.44221112334267,1.6013643061073,4.7692084609066));
#6499=CARTESIAN_POINT('Ctrl Pts',(4.44611558696615,1.56000096824241,4.82404776432428));
#6500=CARTESIAN_POINT('Ctrl Pts',(4.45002028652378,1.51863513092433,4.8788903815043));
#6501=CARTESIAN_POINT('Ctrl Pts',(4.45392498608142,1.4743785176148,4.93154278020563));
#6502=CARTESIAN_POINT('Ctrl Pts',(4.45782968563905,1.42750004749021,4.98169563909031));
#6503=CARTESIAN_POINT('Ctrl Pts',(4.46173853997862,1.38057169649312,5.03190186294942));
#6504=CARTESIAN_POINT('Ctrl Pts',(4.46564739431819,1.33101625765964,5.07960287931854));
#6505=CARTESIAN_POINT('Ctrl Pts',(4.46955624865776,1.27914000413551,5.12452575893484));
#6506=CARTESIAN_POINT('Ctrl Pts',(4.47346744598867,1.22723265566573,5.16947556560168));
#6507=CARTESIAN_POINT('Ctrl Pts',(4.47737864331959,1.17300211219345,5.21164361948917));
#6508=CARTESIAN_POINT('Ctrl Pts',(4.48128984065051,1.11678604131846,5.25079864001233));
#6509=CARTESIAN_POINT('Ctrl Pts',(4.48520777045583,1.06047320384596,5.29002105937809));
#6510=CARTESIAN_POINT('Ctrl Pts',(4.48912570026114,1.00216843533822,5.32621983500999));
#6511=CARTESIAN_POINT('Ctrl Pts',(4.49304363006646,0.942235775033994,5.35920863584006));
#6512=CARTESIAN_POINT('Ctrl Pts',(4.49486099680411,0.914435475194978,5.37451078578218));
#6513=CARTESIAN_POINT('Ctrl Pts',(4.49667836354177,0.886285215289973,5.38912293121047));
#6514=CARTESIAN_POINT('Ctrl Pts',(4.49849573027942,0.857822709676756,5.40303002236758));
#6515=CARTESIAN_POINT('Ctrl Pts',(4.50241422181614,0.796453650230121,5.43301561518745));
#6516=CARTESIAN_POINT('Ctrl Pts',(4.50633271335287,0.73338909294653,5.45983885890346));
#6517=CARTESIAN_POINT('Ctrl Pts',(4.5102512048896,0.668987832150729,5.48330603489983));
#6518=CARTESIAN_POINT('Ctrl Pts',(4.51416380486715,0.604683400411566,5.50673792735539));
#6519=CARTESIAN_POINT('Ctrl Pts',(4.5180764048447,0.539046712223277,5.52682359956585));
#6520=CARTESIAN_POINT('Ctrl Pts',(4.52198900482225,0.472459149121607,5.54341618556753));
#6521=CARTESIAN_POINT('Ctrl Pts',(4.52589701350137,0.405949724182698,5.55998930075327));
#6522=CARTESIAN_POINT('Ctrl Pts',(4.52980502218049,0.338492115304126,5.57307735214722));
#6523=CARTESIAN_POINT('Ctrl Pts',(4.53371303085961,0.270483845284602,5.58258295766677));
#6524=CARTESIAN_POINT('Ctrl Pts',(4.53761859647206,0.202518090200798,5.59208262081772));
#6525=CARTESIAN_POINT('Ctrl Pts',(4.54152416208451,0.134002842795795,5.59800421276478));
#6526=CARTESIAN_POINT('Ctrl Pts',(4.54542972769696,0.0653452906021997,5.60030153033166));
#6527=CARTESIAN_POINT('Ctrl Pts',(4.54933419056062,-0.00329287591447554,
5.60259819924366));
#6528=CARTESIAN_POINT('Ctrl Pts',(4.55323865342427,-0.0720727761918079,
5.60127260884809));
#6529=CARTESIAN_POINT('Ctrl Pts',(4.55714311628792,-0.140584451882745,5.59633059137483));
#6530=CARTESIAN_POINT('Ctrl Pts',(4.56104781508368,-0.209100267478244,5.59138827527393));
#6531=CARTESIAN_POINT('Ctrl Pts',(4.56495251387943,-0.277347336006443,5.5828291361928));
#6532=CARTESIAN_POINT('Ctrl Pts',(4.56885721267518,-0.344919875101811,5.57071094763919));
#6533=CARTESIAN_POINT('Ctrl Pts',(4.57276606625502,-0.4125643145727,5.55857986476018));
#6534=CARTESIAN_POINT('Ctrl Pts',(4.57667491983485,-0.479532307292798,5.54288226179697));
#6535=CARTESIAN_POINT('Ctrl Pts',(4.58058377341469,-0.5454283365702,5.52372704266035));
#6536=CARTESIAN_POINT('Ctrl Pts',(4.584494969986,-0.611363864342917,5.50456034176464));
#6537=CARTESIAN_POINT('Ctrl Pts',(4.58840616655731,-0.676225685518619,5.48193206200187));
#6538=CARTESIAN_POINT('Ctrl Pts',(4.59231736312862,-0.739636199691905,5.45600008922651));
#6539=CARTESIAN_POINT('Ctrl Pts',(4.59623529218249,-0.803155864651535,5.43002347881879));
#6540=CARTESIAN_POINT('Ctrl Pts',(4.60015322123637,-0.865218792240787,5.40073203547598));
#6541=CARTESIAN_POINT('Ctrl Pts',(4.60407115029025,-0.925470798061731,5.3683302026839));
#6542=CARTESIAN_POINT('Ctrl Pts',(4.60588852381033,-0.953419338835413,5.3533002641351));
#6543=CARTESIAN_POINT('Ctrl Pts',(4.60770589733041,-0.980978626059195,5.33760169347744));
#6544=CARTESIAN_POINT('Ctrl Pts',(4.60952327085049,-1.00811553775735,5.32125798199465));
#6545=CARTESIAN_POINT('Ctrl Pts',(4.6134417617717,-1.06662620765759,5.28601883915662));
#6546=CARTESIAN_POINT('Ctrl Pts',(4.6173602526929,-1.12340266514513,5.24763841256609));
#6547=CARTESIAN_POINT('Ctrl Pts',(4.62127874361411,-1.17808737194236,5.20631272915258));
#6548=CARTESIAN_POINT('Ctrl Pts',(4.625191342969,-1.23268985867503,5.16504918011919));
#6549=CARTESIAN_POINT('Ctrl Pts',(4.62910394232389,-1.2852064473077,5.12084945702431));
#6550=CARTESIAN_POINT('Ctrl Pts',(4.63301654167879,-1.33530666907631,5.07395400069755));
#6551=CARTESIAN_POINT('Ctrl Pts',(4.63692454972767,-1.3853480998908,5.0271135746386));
#6552=CARTESIAN_POINT('Ctrl Pts',(4.64083255777656,-1.43297843794731,4.97758403233602));
#6553=CARTESIAN_POINT('Ctrl Pts',(4.64474056582544,-1.47789999451356,4.92564624560195));
#6554=CARTESIAN_POINT('Ctrl Pts',(4.64864613080331,-1.52279346860109,4.87374092750659));
#6555=CARTESIAN_POINT('Ctrl Pts',(4.65255169578118,-1.5649811993835,4.81943072256506));
#6556=CARTESIAN_POINT('Ctrl Pts',(4.65645726075905,-1.60420321923422,4.76303241645459));
#6557=CARTESIAN_POINT('Ctrl Pts',(4.66036172298472,-1.64341416458768,4.70665003463585));
#6558=CARTESIAN_POINT('Ctrl Pts',(4.66426618521039,-1.67966078073795,4.64818112563719));
#6559=CARTESIAN_POINT('Ctrl Pts',(4.66817064743606,-1.71272528491323,4.58797306596664));
#6560=CARTESIAN_POINT('Ctrl Pts',(4.67207534559136,-1.74579178703235,4.52776136818554));
#6561=CARTESIAN_POINT('Ctrl Pts',(4.67598004374666,-1.77567556097404,4.46581074337476));
#6562=CARTESIAN_POINT('Ctrl Pts',(4.67988474190196,-1.80220470312604,4.4024932750836));
#6563=CARTESIAN_POINT('Ctrl Pts',(4.68379359484192,-1.8287620735478,4.33910843399292));
#6564=CARTESIAN_POINT('Ctrl Pts',(4.68770244778188,-1.851957498273,4.27435430137858));
#6565=CARTESIAN_POINT('Ctrl Pts',(4.69161130072184,-1.87166757980071,4.20862211436249));
#6566=CARTESIAN_POINT('Ctrl Pts',(4.69552249665267,-1.89138947567441,4.14285052706291));
#6567=CARTESIAN_POINT('Ctrl Pts',(4.6994336925835,-1.90762175436053,4.07610019650578));
#6568=CARTESIAN_POINT('Ctrl Pts',(4.70334488851433,-1.92029187621531,4.00877392279321));
#6569=CARTESIAN_POINT('Ctrl Pts',(4.70726281693344,-1.93298380762613,3.94133175784014));
#6570=CARTESIAN_POINT('Ctrl Pts',(4.71118074535254,-1.94210127926278,3.8733121582267));
#6571=CARTESIAN_POINT('Ctrl Pts',(4.71509867377164,-1.94762356115874,3.805123552537));
#6572=CARTESIAN_POINT('Ctrl Pts',(4.71691605298829,-1.95018513944007,3.77349343030501));
#6573=CARTESIAN_POINT('Ctrl Pts',(4.71873343220494,-1.95197388355601,3.74182694727269));
#6574=CARTESIAN_POINT('Ctrl Pts',(4.72055081142158,-1.95299152617943,3.71016467356758));
#6575=CARTESIAN_POINT('Ctrl Pts',(4.72174397690631,-1.95365963993518,3.68937741474617));
#6576=CARTESIAN_POINT('Ctrl Pts',(4.72293714239104,-1.95399588157958,3.66857943228897));
#6577=CARTESIAN_POINT('Ctrl Pts',(4.72413030787577,-1.95399996239942,3.64777779982395));
#6578=CARTESIAN_POINT('Origin',(0.,0.,3.64739446828387));
#6579=CARTESIAN_POINT('',(5.5258696920781,-1.95399938884984,3.64893990493634));
#6580=CARTESIAN_POINT('',(5.42413030787577,-1.95399943981962,3.64887405762318));
#6581=CARTESIAN_POINT('',(0.,-1.954,3.64739446828387));
#6582=CARTESIAN_POINT('Ctrl Pts',(5.5258696920781,-1.95399938884984,3.64893990493634));
#6583=CARTESIAN_POINT('Ctrl Pts',(5.5212902068915,-1.9539356881594,3.72948096754407));
#6584=CARTESIAN_POINT('Ctrl Pts',(5.5167107217049,-1.9488883727995,3.80981306186029));
#6585=CARTESIAN_POINT('Ctrl Pts',(5.5121312365183,-1.93895808420072,3.88938113674448));
#6586=CARTESIAN_POINT('Ctrl Pts',(5.50750036886044,-1.92891637635988,3.96984197667854));
#6587=CARTESIAN_POINT('Ctrl Pts',(5.50286950120259,-1.91388160449041,4.04952144814043));
#6588=CARTESIAN_POINT('Ctrl Pts',(5.49823863354473,-1.89400709304308,4.12786624841512));
#6589=CARTESIAN_POINT('Ctrl Pts',(5.49540062045956,-1.8818270594692,4.17587961972306));
#6590=CARTESIAN_POINT('Ctrl Pts',(5.49256260737439,-1.86783026256677,4.22339212396149));
#6591=CARTESIAN_POINT('Ctrl Pts',(5.48972459428922,-1.85206076918552,4.27028041871455));
#6592=CARTESIAN_POINT('Ctrl Pts',(5.48580620372998,-1.83028813032352,4.33501819334261));
#6593=CARTESIAN_POINT('Ctrl Pts',(5.48188781317074,-1.80507401469032,4.3987411113528));
#6594=CARTESIAN_POINT('Ctrl Pts',(5.4779694226115,-1.77653259424169,4.46105775343129));
#6595=CARTESIAN_POINT('Ctrl Pts',(5.4740569252752,-1.74803409982388,4.52328067185987));
#6596=CARTESIAN_POINT('Ctrl Pts',(5.4701444279389,-1.71621843543999,4.58410106841765));
#6597=CARTESIAN_POINT('Ctrl Pts',(5.46623193060261,-1.681248985294,4.64314436130314));
#6598=CARTESIAN_POINT('Ctrl Pts',(5.46232402652118,-1.64632058913045,4.70211833761949));
#6599=CARTESIAN_POINT('Ctrl Pts',(5.45841612243974,-1.6082460099648,4.75931893258282));
#6600=CARTESIAN_POINT('Ctrl Pts',(5.45450821835831,-1.56723518853569,4.81439483838471));
#6601=CARTESIAN_POINT('Ctrl Pts',(5.45060275849708,-1.5262500175515,4.86943629665693));
#6602=CARTESIAN_POINT('Ctrl Pts',(5.44669729863585,-1.48233254040954,4.92235530833337));
#6603=CARTESIAN_POINT('Ctrl Pts',(5.44279183877463,-1.43573591095844,4.97282963983483));
#6604=CARTESIAN_POINT('Ctrl Pts',(5.43888748265438,-1.38915245040719,5.02328970654023));
#6605=CARTESIAN_POINT('Ctrl Pts',(5.43498312653414,-1.33989167411582,5.07130610346443));
#6606=CARTESIAN_POINT('Ctrl Pts',(5.4310787704139,-1.28824571546202,5.11659117961757));
#6607=CARTESIAN_POINT('Ctrl Pts',(5.42717417919354,-1.23659664695582,5.16187898260368));
#6608=CARTESIAN_POINT('Ctrl Pts',(5.42326958797317,-1.182562482418,5.20443481600184));
#6609=CARTESIAN_POINT('Ctrl Pts',(5.41936499675281,-1.12646938739021,5.24401048952151));
#6610=CARTESIAN_POINT('Ctrl Pts',(5.41545625127246,-1.07031661254271,5.28362826927653));
#6611=CARTESIAN_POINT('Ctrl Pts',(5.41154750579211,-1.0121009381428,5.32025927739807));
#6612=CARTESIAN_POINT('Ctrl Pts',(5.40763876031176,-0.952177706508478,5.35369854881238));
#6613=CARTESIAN_POINT('Ctrl Pts',(5.40372767229675,-0.892218562521245,5.38715786058306));
#6614=CARTESIAN_POINT('Ctrl Pts',(5.39981658428174,-0.830550266193544,5.41742141207729));
#6615=CARTESIAN_POINT('Ctrl Pts',(5.39590549626673,-0.767550432645577,5.44433139910409));
#6616=CARTESIAN_POINT('Ctrl Pts',(5.39198767533847,-0.704442145283215,5.4712877115031));
#6617=CARTESIAN_POINT('Ctrl Pts',(5.38806985441022,-0.639998207400958,5.49487876839444));
#6618=CARTESIAN_POINT('Ctrl Pts',(5.38415203348196,-0.574612917818897,5.51499613745095));
#6619=CARTESIAN_POINT('Ctrl Pts',(5.38233370689402,-0.544266505186804,5.52433294679083));
#6620=CARTESIAN_POINT('Ctrl Pts',(5.38051538030607,-0.513717484252054,5.53292222715614));
#6621=CARTESIAN_POINT('Ctrl Pts',(5.37869705371813,-0.483005906313095,5.54075689911075));
#6622=CARTESIAN_POINT('Ctrl Pts',(5.3747785277876,-0.41682191311884,5.55764075562746));
#6623=CARTESIAN_POINT('Ctrl Pts',(5.37086000185706,-0.349620703532015,5.57108354879798));
#6624=CARTESIAN_POINT('Ctrl Pts',(5.36694147592653,-0.28179296869672,5.58096854826971));
#6625=CARTESIAN_POINT('Ctrl Pts',(5.36302884120956,-0.214067207837933,5.59083868637675));
#6626=CARTESIAN_POINT('Ctrl Pts',(5.35911620649258,-0.145717273873157,5.59716157616642));
#6627=CARTESIAN_POINT('Ctrl Pts',(5.35520357177561,-0.0771464480078521,
5.59987095356091));
#6628=CARTESIAN_POINT('Ctrl Pts',(5.35129552801878,-0.0086560809513348,
5.60257715185882));
#6629=CARTESIAN_POINT('Ctrl Pts',(5.34738748426195,0.0600541741938194,5.60167823916572));
#6630=CARTESIAN_POINT('Ctrl Pts',(5.34347944050512,0.128575292284431,5.59715968343516));
#6631=CARTESIAN_POINT('Ctrl Pts',(5.33957383962591,0.19705357853482,5.59264395220693));
#6632=CARTESIAN_POINT('Ctrl Pts',(5.3356682387467,0.265342472664014,5.58451309856252));
#6633=CARTESIAN_POINT('Ctrl Pts',(5.33176263786749,0.333033891361192,5.57280466541196));
#6634=CARTESIAN_POINT('Ctrl Pts',(5.32785813960241,0.40070619967885,5.56109953774096));
#6635=CARTESIAN_POINT('Ctrl Pts',(5.32395364133733,0.467780883087807,5.54581891941337));
#6636=CARTESIAN_POINT('Ctrl Pts',(5.32004914307226,0.533857724051826,5.52705186538319));
#6637=CARTESIAN_POINT('Ctrl Pts',(5.31614440879464,0.599938559117517,5.50828367695372));
#6638=CARTESIAN_POINT('Ctrl Pts',(5.31223967451703,0.665020959650779,5.48602877125562));
#6639=CARTESIAN_POINT('Ctrl Pts',(5.30833494023941,0.728719356347928,5.46042621088626));
#6640=CARTESIAN_POINT('Ctrl Pts',(5.30442605130004,0.792485528538487,5.43479640923217));
#6641=CARTESIAN_POINT('Ctrl Pts',(5.30051716236068,0.854864300948419,5.40581202823348));
#6642=CARTESIAN_POINT('Ctrl Pts',(5.29660827342131,0.915490550093816,5.37366010621128));
#6643=CARTESIAN_POINT('Ctrl Pts',(5.29269704150905,0.976153138378216,5.34148891245151));
#6644=CARTESIAN_POINT('Ctrl Pts',(5.28878580959679,1.03506069105752,5.30614665209333));
#6645=CARTESIAN_POINT('Ctrl Pts',(5.28487457768453,1.09187558439379,5.26786468035342));
#6646=CARTESIAN_POINT('Ctrl Pts',(5.28095661368922,1.14878826855117,5.22951681699196));
#6647=CARTESIAN_POINT('Ctrl Pts',(5.27703864969391,1.2036007120853,5.18821943943023));
#6648=CARTESIAN_POINT('Ctrl Pts',(5.2731206856986,1.25600768300813,5.14424472807092));
#6649=CARTESIAN_POINT('Ctrl Pts',(5.27130362818142,1.28031277631217,5.12385031404954));
#6650=CARTESIAN_POINT('Ctrl Pts',(5.26948657066424,1.30410099538047,5.10288056396185));
#6651=CARTESIAN_POINT('Ctrl Pts',(5.26766951314706,1.32734469991678,5.08136519588009));
#6652=CARTESIAN_POINT('Ctrl Pts',(5.2637510139676,1.37746993607034,5.03496713121943));
#6653=CARTESIAN_POINT('Ctrl Pts',(5.25983251478814,1.42525856221545,4.98584591761485));
#6654=CARTESIAN_POINT('Ctrl Pts',(5.25591401560868,1.47040035663306,4.93426617564765));
#6655=CARTESIAN_POINT('Ctrl Pts',(5.25200140773905,1.51547428213322,4.88276398179955));
#6656=CARTESIAN_POINT('Ctrl Pts',(5.24808879986942,1.55790895241809,4.82881096259536));
#6657=CARTESIAN_POINT('Ctrl Pts',(5.2441761919998,1.59742967920941,4.77270972188214));
#6658=CARTESIAN_POINT('Ctrl Pts',(5.24026817509748,1.63690403325633,4.71667430912065));
#6659=CARTESIAN_POINT('Ctrl Pts',(5.23636015819516,1.67347095248099,4.6584960811169));
#6660=CARTESIAN_POINT('Ctrl Pts',(5.23245214129284,1.70689606355718,4.59851056435891));
#6661=CARTESIAN_POINT('Ctrl Pts',(5.22854656725618,1.74030028090181,4.53856254399939));
#6662=CARTESIAN_POINT('Ctrl Pts',(5.22464099321952,1.77056634709305,4.47680990453244));
#6663=CARTESIAN_POINT('Ctrl Pts',(5.22073541918286,1.79750412333855,4.41361566779541));
#6664=CARTESIAN_POINT('Ctrl Pts',(5.21683094770655,1.82443429493397,4.3504392710632));
#6665=CARTESIAN_POINT('Ctrl Pts',(5.21292647623023,1.84803784911861,4.28582253714588));
#6666=CARTESIAN_POINT('Ctrl Pts',(5.20902200475392,1.86817217000137,4.2201498639218));
#6667=CARTESIAN_POINT('Ctrl Pts',(5.20511729716942,1.88830770843128,4.15447321939041));
#6668=CARTESIAN_POINT('Ctrl Pts',(5.20121258958492,1.90497345537369,4.08774097969503));
#6669=CARTESIAN_POINT('Ctrl Pts',(5.19730788200041,1.91807673883901,4.02035240683018));
#6670=CARTESIAN_POINT('Ctrl Pts',(5.19339901942455,1.93119396548149,3.95289212592267));
#6671=CARTESIAN_POINT('Ctrl Pts',(5.18949015684869,1.94074106941273,3.88477460170885));
#6672=CARTESIAN_POINT('Ctrl Pts',(5.18558129427282,1.94667676563991,3.81640798880139));
#6673=CARTESIAN_POINT('Ctrl Pts',(5.18167008857389,1.95261601995246,3.74800039430797));
#6674=CARTESIAN_POINT('Ctrl Pts',(5.17775888287496,1.95493954153139,3.67934390549881));
#6675=CARTESIAN_POINT('Ctrl Pts',(5.17384767717603,1.95365819189621,3.610847659438));
#6676=CARTESIAN_POINT('Ctrl Pts',(5.16992973888634,1.95237463659778,3.54223350671916));
#6677=CARTESIAN_POINT('Ctrl Pts',(5.16601180059666,1.94747386063337,3.47378063748742));
#6678=CARTESIAN_POINT('Ctrl Pts',(5.16209386230698,1.93901859753385,3.40589316721522));
#6679=CARTESIAN_POINT('Ctrl Pts',(5.16027656572998,1.93509670812358,3.37440424160557));
#6680=CARTESIAN_POINT('Ctrl Pts',(5.15845926915297,1.93041080123306,3.34303681436164));
#6681=CARTESIAN_POINT('Ctrl Pts',(5.15664197257597,1.92497081948355,3.31183025067891));
#6682=CARTESIAN_POINT('Ctrl Pts',(5.1527234949001,1.91324106259501,3.24454226660472));
#6683=CARTESIAN_POINT('Ctrl Pts',(5.14880501722423,1.89795575006274,3.17773696910643));
#6684=CARTESIAN_POINT('Ctrl Pts',(5.14488653954836,1.87916855139227,3.11181855820361));
#6685=CARTESIAN_POINT('Ctrl Pts',(5.1409739536715,1.86040960103854,3.04599926181934));
#6686=CARTESIAN_POINT('Ctrl Pts',(5.13706136779464,1.83815934832929,2.98106467459703));
#6687=CARTESIAN_POINT('Ctrl Pts',(5.13314878191778,1.81252265527333,2.91740979438932));
#6688=CARTESIAN_POINT('Ctrl Pts',(5.1292407876249,1.78691604795422,2.85382961585905));
#6689=CARTESIAN_POINT('Ctrl Pts',(5.12533279333202,1.75793107587759,2.79152661575932));
#6690=CARTESIAN_POINT('Ctrl Pts',(5.12142479903914,1.72572214182346,2.73087982616392));
#6691=CARTESIAN_POINT('Ctrl Pts',(5.11751924798183,1.69353334444492,2.6702709522824));
#6692=CARTESIAN_POINT('Ctrl Pts',(5.11361369692452,1.65812481356218,2.61131666823854));
#6693=CARTESIAN_POINT('Ctrl Pts',(5.10970814586721,1.61969806496519,2.55437380134843));
#6694=CARTESIAN_POINT('Ctrl Pts',(5.10580369770541,1.58128216776612,2.49744701465582));
#6695=CARTESIAN_POINT('Ctrl Pts',(5.10189924954361,1.53985001983801,2.44253092495091));
#6696=CARTESIAN_POINT('Ctrl Pts',(5.09799480138181,1.49564689828914,2.38995406984024));
#6697=CARTESIAN_POINT('Ctrl Pts',(5.09409011741262,1.45144110711252,2.33737403937394));
#6698=CARTESIAN_POINT('Ctrl Pts',(5.09018543344342,1.40446432849761,2.28713389874035));
#6699=CARTESIAN_POINT('Ctrl Pts',(5.08628074947422,1.35500144837195,2.23952832588612));
#6700=CARTESIAN_POINT('Ctrl Pts',(5.08237191080845,1.30548593831249,2.1918720993267));
#6701=CARTESIAN_POINT('Ctrl Pts',(5.07846307214267,1.25347940263475,2.14685637657938));
#6702=CARTESIAN_POINT('Ctrl Pts',(5.0745542334769,1.19930210612833,2.10473752060038));
#6703=CARTESIAN_POINT('Ctrl Pts',(5.07064305189136,1.14509233627887,2.06259341898996));
#6704=CARTESIAN_POINT('Ctrl Pts',(5.06673187030582,1.08870961977553,2.0233499207839));
#6705=CARTESIAN_POINT('Ctrl Pts',(5.06282068872027,1.03050337127767,1.98722013955048));
#6706=CARTESIAN_POINT('Ctrl Pts',(5.05890277460612,0.972196929213073,1.95102816616862));
#6707=CARTESIAN_POINT('Ctrl Pts',(5.05498486049197,0.912061121091883,1.91796084372818));
#6708=CARTESIAN_POINT('Ctrl Pts',(5.05106694637782,0.85046932120423,1.8881850055733));
#6709=CARTESIAN_POINT('Ctrl Pts',(5.04924944158685,0.821897129951701,1.87437211255804));
#6710=CARTESIAN_POINT('Ctrl Pts',(5.04743193679588,0.793011879616,1.86126686004469));
#6711=CARTESIAN_POINT('Ctrl Pts',(5.0456144320049,0.763852036129499,1.84888228681252));
#6712=CARTESIAN_POINT('Ctrl Pts',(5.04169593494842,0.700984107837442,1.82218144178747));
#6713=CARTESIAN_POINT('Ctrl Pts',(5.03777743789193,0.636590155551074,1.79872813327964));
#6714=CARTESIAN_POINT('Ctrl Pts',(5.03385894083545,0.571038710239964,1.77869684924341));
#6715=CARTESIAN_POINT('Ctrl Pts',(5.02994633527566,0.505585822135272,1.75869568242865));
#6716=CARTESIAN_POINT('Ctrl Pts',(5.02603372971586,0.438979361448329,1.74210647146395));
#6717=CARTESIAN_POINT('Ctrl Pts',(5.02212112415607,0.371607938864396,1.72905572349114));
#6718=CARTESIAN_POINT('Ctrl Pts',(5.01821310983003,0.304315573048273,1.71602028987436));
#6719=CARTESIAN_POINT('Ctrl Pts',(5.01430509550399,0.236260508593107,1.70651516594548));
#6720=CARTESIAN_POINT('Ctrl Pts',(5.01039708117795,0.167844859934864,1.70061659112545));
#6721=CARTESIAN_POINT('Ctrl Pts',(5.00649150988179,0.0994719801766054,1.69472170370094));
#6722=CARTESIAN_POINT('Ctrl Pts',(5.00258593858563,0.0307394522219118,1.69242893512387));
#6723=CARTESIAN_POINT('Ctrl Pts',(4.99868036728947,-0.0379436627796898,
1.69376290669022));
#6724=CARTESIAN_POINT('Ctrl Pts',(4.99477589871406,-0.106607385407976,1.6950965016156));
#6725=CARTESIAN_POINT('Ctrl Pts',(4.99087143013866,-0.175221231337169,1.70005479430132));
#6726=CARTESIAN_POINT('Ctrl Pts',(4.98696696156326,-0.243376122230716,1.70861029692081));
#6727=CARTESIAN_POINT('Ctrl Pts',(4.98306225703643,-0.31153513180085,1.71716631655894));
#6728=CARTESIAN_POINT('Ctrl Pts',(4.97915755250961,-0.379234643660647,1.72931991390672));
#6729=CARTESIAN_POINT('Ctrl Pts',(4.97525284798278,-0.446072494380595,1.74499195310548));
#6730=CARTESIAN_POINT('Ctrl Pts',(4.97134398868202,-0.512981463454875,1.76068066802951));
#6731=CARTESIAN_POINT('Ctrl Pts',(4.96743512938126,-0.579026461982407,1.77989518365212));
#6732=CARTESIAN_POINT('Ctrl Pts',(4.9635262700805,-0.643818279759126,1.80250584762191));
#6733=CARTESIAN_POINT('Ctrl Pts',(4.95961506778575,-0.708648934144592,1.82513006456089));
#6734=CARTESIAN_POINT('Ctrl Pts',(4.95570386549101,-0.772224457656741,1.85115429490041));
#6735=CARTESIAN_POINT('Ctrl Pts',(4.95179266319626,-0.834176119683401,1.88040091952656));
#6736=CARTESIAN_POINT('Ctrl Pts',(4.94787472847511,-0.896234420276364,1.90969788692024));
#6737=CARTESIAN_POINT('Ctrl Pts',(4.94395679375397,-0.956662847974479,1.94222808592322));
#6738=CARTESIAN_POINT('Ctrl Pts',(4.94003885903282,-1.01511851568075,1.97776864220124));
#6739=CARTESIAN_POINT('Ctrl Pts',(4.93822153649982,-1.04223300575396,1.99425402502569));
#6740=CARTESIAN_POINT('Ctrl Pts',(4.93640421396682,-1.06892347732316,2.01138649999384));
#6741=CARTESIAN_POINT('Ctrl Pts',(4.93458689143382,-1.09515809873353,2.02914086060109));
#6742=CARTESIAN_POINT('Ctrl Pts',(4.93068215939183,-1.15152628047912,2.06728820070679));
#6743=CARTESIAN_POINT('Ctrl Pts',(4.92677742734985,-1.20601427441912,2.10846238665924));
#6744=CARTESIAN_POINT('Ctrl Pts',(4.92287269530787,-1.25827678983217,2.15245115157596));
#6745=CARTESIAN_POINT('Ctrl Pts',(4.91883090350855,-1.31237376855875,2.19798396340297));
#6746=CARTESIAN_POINT('Ctrl Pts',(4.91478911170923,-1.36408562775221,2.24653241326184));
#6747=CARTESIAN_POINT('Ctrl Pts',(4.91074731990991,-1.41306090869161,2.2978112480534));
#6748=CARTESIAN_POINT('Ctrl Pts',(4.90685312352861,-1.46024774346118,2.34721751705428));
#6749=CARTESIAN_POINT('Ctrl Pts',(4.90295892714731,-1.50489402519348,2.39915781793863));
#6750=CARTESIAN_POINT('Ctrl Pts',(4.89906473076601,-1.54671985078526,2.45333680502517));
#6751=CARTESIAN_POINT('Ctrl Pts',(4.8951728750249,-1.58852053660526,2.50748322736611));
#6752=CARTESIAN_POINT('Ctrl Pts',(4.89128101928378,-1.62750382633117,2.56386527560233));
#6753=CARTESIAN_POINT('Ctrl Pts',(4.88738916354267,-1.66342951017403,2.6221538796013));
#6754=CARTESIAN_POINT('Ctrl Pts',(4.88349828789472,-1.69934614678601,2.68042780467419));
#6755=CARTESIAN_POINT('Ctrl Pts',(4.87960741224678,-1.7322064461976,2.74060691051924));
#6756=CARTESIAN_POINT('Ctrl Pts',(4.87571653659884,-1.7618140741168,2.80233401586407));
#6757=CARTESIAN_POINT('Ctrl Pts',(4.87182528202397,-1.79142458548136,2.86406713272511));
#6758=CARTESIAN_POINT('Ctrl Pts',(4.86793402744911,-1.81778158504715,2.92734810008857));
#6759=CARTESIAN_POINT('Ctrl Pts',(4.86404277287425,-1.84073598285885,2.9917977619097));
#6760=CARTESIAN_POINT('Ctrl Pts',(4.86014733215933,-1.86371507458922,3.05631675749073));
#6761=CARTESIAN_POINT('Ctrl Pts',(4.85625189144442,-1.88328409647481,3.12200648773817));
#6762=CARTESIAN_POINT('Ctrl Pts',(4.85235645072951,-1.89934352177914,3.18847161390025));
#6763=CARTESIAN_POINT('Ctrl Pts',(4.84845849903485,-1.91541329890106,3.25497958311862));
#6764=CARTESIAN_POINT('Ctrl Pts',(4.84456054734019,-1.92796888898619,3.32226345550716));
#6765=CARTESIAN_POINT('Ctrl Pts',(4.84066259564552,-1.93696221203219,3.389919442001));
#6766=CARTESIAN_POINT('Ctrl Pts',(4.83675820641697,-1.94597038770502,3.45768716351374));
#6767=CARTESIAN_POINT('Ctrl Pts',(4.83285381718841,-1.95140452392265,3.52582773192013));
#6768=CARTESIAN_POINT('Ctrl Pts',(4.82894942795985,-1.95326856711039,3.59393509362883));
#6769=CARTESIAN_POINT('Ctrl Pts',(4.82792284934798,-1.95375867881702,3.61184251954066));
#6770=CARTESIAN_POINT('Ctrl Pts',(4.8268962707361,-1.95400226243369,3.62974767089812));
#6771=CARTESIAN_POINT('Ctrl Pts',(4.82586969212423,-1.95399998416516,3.64764323036849));
#6772=CARTESIAN_POINT('Ctrl Pts',(4.72413079030316,-1.95710318190607,3.64776998461592));
#6773=CARTESIAN_POINT('Ctrl Pts',(4.75994664419966,-1.9554136014585,3.022364796511));
#6774=CARTESIAN_POINT('Ctrl Pts',(4.8327716782865,-1.29210840943672,1.74764265246943));
#6775=CARTESIAN_POINT('Ctrl Pts',(4.94260589256374,0.878268351030341,1.51220654580568));
#6776=CARTESIAN_POINT('Ctrl Pts',(5.05363343313481,2.26979830067418,3.22502187308483));
#6777=CARTESIAN_POINT('Ctrl Pts',(5.16466097370589,1.5875322833648,5.32373643149222));
#6778=CARTESIAN_POINT('Ctrl Pts',(5.27568851427697,-0.545177970067405,5.8908661531987));
#6779=CARTESIAN_POINT('Ctrl Pts',(5.36217802636002,-1.81852615233383,4.735922224886));
#6780=CARTESIAN_POINT('Ctrl Pts',(5.41165835825273,-1.95368429139157,3.8680854635217));
#6781=CARTESIAN_POINT('Ctrl Pts',(5.42412950995508,-1.95213885961564,3.64888667332463));
#6782=CARTESIAN_POINT('Origin',(0.,0.,3.64739446828387));
#6783=CARTESIAN_POINT('',(6.22586985342116,-1.95353597714873,3.64632535240864));
#6784=CARTESIAN_POINT('',(6.12413030792735,-1.95399955699052,3.64607868681971));
#6785=CARTESIAN_POINT('',(0.,-1.954,3.64739446828387));
#6786=CARTESIAN_POINT('Ctrl Pts',(6.22586969212423,-1.95399970893239,3.64632793551611));
#6787=CARTESIAN_POINT('Ctrl Pts',(6.22192922025797,-1.95403757522788,3.71570295389058));
#6788=CARTESIAN_POINT('Ctrl Pts',(6.21798874839172,-1.95037645685081,3.78509205096179));
#6789=CARTESIAN_POINT('Ctrl Pts',(6.21404827652546,-1.94303829200873,3.85407827458662));
#6790=CARTESIAN_POINT('Ctrl Pts',(6.21010723418459,-1.93569906479724,3.92307448556594));
#6791=CARTESIAN_POINT('Ctrl Pts',(6.20616619184372,-1.92468178589053,3.9916672306491));
#6792=CARTESIAN_POINT('Ctrl Pts',(6.20222514950284,-1.91006015343086,4.05944569116239));
#6793=CARTESIAN_POINT('Ctrl Pts',(6.19827911405417,-1.89541999607833,4.12731002366864));
#6794=CARTESIAN_POINT('Ctrl Pts',(6.19433307860549,-1.87716646696284,4.19435754146509));
#6795=CARTESIAN_POINT('Ctrl Pts',(6.19038704315681,-1.8554240829409,4.26018927280079));
#6796=CARTESIAN_POINT('Ctrl Pts',(6.1864385391419,-1.83366809728873,4.32606218724066));
#6797=CARTESIAN_POINT('Ctrl Pts',(6.182490035127,-1.80841908414581,4.39071735315625));
#6798=CARTESIAN_POINT('Ctrl Pts',(6.17854153111209,-1.77984999050235,4.45377527863887));
#6799=CARTESIAN_POINT('Ctrl Pts',(6.17458487851165,-1.75122193840214,4.51696333768535));
#6800=CARTESIAN_POINT('Ctrl Pts',(6.1706282259112,-1.71926033568415,4.57854714271377));
#6801=CARTESIAN_POINT('Ctrl Pts',(6.16667157331076,-1.68418427929637,4.6381715942668));
#6802=CARTESIAN_POINT('Ctrl Pts',(6.16307766144574,-1.65232394988149,4.69232975408553));
#6803=CARTESIAN_POINT('Ctrl Pts',(6.15948374958071,-1.61789476739727,4.74487148430732));
#6804=CARTESIAN_POINT('Ctrl Pts',(6.15588983771569,-1.58109015814158,4.79555382648631));
#6805=CARTESIAN_POINT('Ctrl Pts',(6.15197641278596,-1.54101347268034,4.85074203054616));
#6806=CARTESIAN_POINT('Ctrl Pts',(6.14806298785624,-1.49796252247789,4.90394126259883));
#6807=CARTESIAN_POINT('Ctrl Pts',(6.14414956292652,-1.45216195437606,4.95481240385869));
#6808=CARTESIAN_POINT('Ctrl Pts',(6.1402421044734,-1.40643121462739,5.00560598608019));
#6809=CARTESIAN_POINT('Ctrl Pts',(6.13633464602028,-1.35795950337581,5.0540781577686));
#6810=CARTESIAN_POINT('Ctrl Pts',(6.13242718756716,-1.30701347514826,5.09992046659883));
#6811=CARTESIAN_POINT('Ctrl Pts',(6.12852440627108,-1.25612842839426,5.14570790301524));
#6812=CARTESIAN_POINT('Ctrl Pts',(6.12462162497499,-1.20277531117033,5.18887139966881));
#6813=CARTESIAN_POINT('Ctrl Pts',(6.12071884367891,-1.14725832432906,5.22913854911922));
#6814=CARTESIAN_POINT('Ctrl Pts',(6.11681855583622,-1.09177680681312,5.26937997223424));
#6815=CARTESIAN_POINT('Ctrl Pts',(6.11291826799353,-1.03413456015337,5.30672842959029));
#6816=CARTESIAN_POINT('Ctrl Pts',(6.10901798015085,-0.974668408497115,5.34095211226228));
#6817=CARTESIAN_POINT('Ctrl Pts',(6.10511883754132,-0.915219717759566,5.37516574590766));
#6818=CARTESIAN_POINT('Ctrl Pts',(6.1012196949318,-0.853948612355486,5.40625618021191));
#6819=CARTESIAN_POINT('Ctrl Pts',(6.09732055232227,-0.791218844617588,5.4340362174664));
#6820=CARTESIAN_POINT('Ctrl Pts',(6.09342120841215,-0.728485838336974,5.46181768891777));
#6821=CARTESIAN_POINT('Ctrl Pts',(6.08952186450202,-0.664294472261642,5.48628822667262));
#6822=CARTESIAN_POINT('Ctrl Pts',(6.0856225205919,-0.599029234794682,5.50730843830004));
#6823=CARTESIAN_POINT('Ctrl Pts',(6.08171903797274,-0.533694725718389,5.52835096048579));
#6824=CARTESIAN_POINT('Ctrl Pts',(6.07781555535358,-0.467284540994088,5.54593569663872));
#6825=CARTESIAN_POINT('Ctrl Pts',(6.07391207273442,-0.400198132893067,5.55997321291869));
#6826=CARTESIAN_POINT('Ctrl Pts',(6.07000626427478,-0.333071752208878,5.57401909327423));
#6827=CARTESIAN_POINT('Ctrl Pts',(6.06610045581514,-0.265268833825991,5.58451347230018));
#6828=CARTESIAN_POINT('Ctrl Pts',(6.0621946473555,-0.19719600918756,5.59141857666332));
#6829=CARTESIAN_POINT('Ctrl Pts',(6.0582820765205,-0.129005325725104,5.59833563627416));
#6830=CARTESIAN_POINT('Ctrl Pts',(6.0543695056855,-0.0605442957425206,5.60165099501344));
#6831=CARTESIAN_POINT('Ctrl Pts',(6.0504569348505,0.00777927282227454,5.60137898278606));
#6832=CARTESIAN_POINT('Ctrl Pts',(6.0485920556152,0.0403448696309175,5.60124933147086));
#6833=CARTESIAN_POINT('Ctrl Pts',(6.04672717637991,0.0728792977294585,5.60030545174069));
#6834=CARTESIAN_POINT('Ctrl Pts',(6.04486229714461,0.105338970147309,5.59855302190485));
#6835=CARTESIAN_POINT('Ctrl Pts',(6.0409427454772,0.173561813075101,5.59486981327929));
#6836=CARTESIAN_POINT('Ctrl Pts',(6.03702319380979,0.241725674141686,5.58759689429554));
#6837=CARTESIAN_POINT('Ctrl Pts',(6.03310364214238,0.309422647204876,5.57673985607651));
#6838=CARTESIAN_POINT('Ctrl Pts',(6.02918997732355,0.377017944907487,5.56589912424794));
#6839=CARTESIAN_POINT('Ctrl Pts',(6.02527631250471,0.444147264941309,5.55148503414074));
#6840=CARTESIAN_POINT('Ctrl Pts',(6.02136264768587,0.510405798910706,5.53355509782694));
#6841=CARTESIAN_POINT('Ctrl Pts',(6.01745357256907,0.576586629003434,5.51564618862432));
#6842=CARTESIAN_POINT('Ctrl Pts',(6.01354449745227,0.641898229039043,5.494229749871));
#6843=CARTESIAN_POINT('Ctrl Pts',(6.00963542233547,0.705945795963414,5.46941437299446));
#6844=CARTESIAN_POINT('Ctrl Pts',(6.00572878995174,0.769953340349117,5.44461450294243));
#6845=CARTESIAN_POINT('Ctrl Pts',(6.00182215756802,0.832697961298201,5.4164200853168));
#6846=CARTESIAN_POINT('Ctrl Pts',(5.99791552518429,0.893801338935865,5.38498911794082));
#6847=CARTESIAN_POINT('Ctrl Pts',(5.9940099968832,0.954887447690414,5.35356703350589));
#6848=CARTESIAN_POINT('Ctrl Pts',(5.9901044685821,1.01433279715154,5.31891043993515));
#6849=CARTESIAN_POINT('Ctrl Pts',(5.98619894028101,1.07178198514831,5.28122413391966));
#6850=CARTESIAN_POINT('Ctrl Pts',(5.98229317904975,1.12923459948019,5.24353558024988));
#6851=CARTESIAN_POINT('Ctrl Pts',(5.97838741781849,1.18469040646371,5.20281722710309));
#6852=CARTESIAN_POINT('Ctrl Pts',(5.97448165658724,1.23782293994471,5.15931720749597));
#6853=CARTESIAN_POINT('Ctrl Pts',(5.97057175247585,1.29101183163716,5.11577104698155));
#6854=CARTESIAN_POINT('Ctrl Pts',(5.96666184836446,1.34187215084874,5.06943764360154));
#6855=CARTESIAN_POINT('Ctrl Pts',(5.96275194425307,1.39011129021969,5.02060479478297));
#6856=CARTESIAN_POINT('Ctrl Pts',(5.95883970243907,1.4383792714135,4.97174274916706));
#6857=CARTESIAN_POINT('Ctrl Pts',(5.95492746062508,1.48402262717616,4.92037865129621));
#6858=CARTESIAN_POINT('Ctrl Pts',(5.95101521881108,1.52678824140369,4.86683436672554));
#6859=CARTESIAN_POINT('Ctrl Pts',(5.94709626367075,1.56962724054399,4.81319820126589));
#6860=CARTESIAN_POINT('Ctrl Pts',(5.94317730853042,1.60957835661113,4.75737478184438));
#6861=CARTESIAN_POINT('Ctrl Pts',(5.93925835339009,1.64643158878359,4.69971524801576));
#6862=CARTESIAN_POINT('Ctrl Pts',(5.93745048778457,1.66343247001623,4.67311614588104));
#6863=CARTESIAN_POINT('Ctrl Pts',(5.93564262217905,1.67977473443783,4.64612664650916));
#6864=CARTESIAN_POINT('Ctrl Pts',(5.93383475657353,1.69544115163435,4.61878280532771));
#6865=CARTESIAN_POINT('Ctrl Pts',(5.9299154907718,1.72940432509505,4.55950418345275));
#6866=CARTESIAN_POINT('Ctrl Pts',(5.92599622497008,1.76032172067738,4.49832553361446));
#6867=CARTESIAN_POINT('Ctrl Pts',(5.92207695916835,1.78797652885593,4.43559236999402));
#6868=CARTESIAN_POINT('Ctrl Pts',(5.91816356697678,1.81558989213881,4.37295322146871));
#6869=CARTESIAN_POINT('Ctrl Pts',(5.91425017478521,1.83995017544407,4.30876462905164));
#6870=CARTESIAN_POINT('Ctrl Pts',(5.91033678259365,1.86088584978546,4.24339770155383));
#6871=CARTESIAN_POINT('Ctrl Pts',(5.90642795900979,1.88179708321256,4.17810708530575));
#6872=CARTESIAN_POINT('Ctrl Pts',(5.90251913542593,1.89929149862642,4.11164133195098));
#6873=CARTESIAN_POINT('Ctrl Pts',(5.89861031184207,1.91324589168177,4.04439088887583));
#6874=CARTESIAN_POINT('Ctrl Pts',(5.89470391770692,1.92719161167183,3.97718224392699));
#6875=CARTESIAN_POINT('Ctrl Pts',(5.89079752357176,1.93760157433054,3.90919035696604));
#6876=CARTESIAN_POINT('Ctrl Pts',(5.88689112943661,1.94440301405621,3.84081866255422));
#6877=CARTESIAN_POINT('Ctrl Pts',(5.8829858256886,1.9512025553041,3.77246605265203));
#6878=CARTESIAN_POINT('Ctrl Pts',(5.87908052194059,1.95439552460934,3.70373433466594));
#6879=CARTESIAN_POINT('Ctrl Pts',(5.87517521819257,1.95396089951249,3.63503311009168));
#6880=CARTESIAN_POINT('Ctrl Pts',(5.87126966739349,1.95352624692107,3.56632753945049));
#6881=CARTESIAN_POINT('Ctrl Pts',(5.8673641165944,1.94946355000497,3.49765295755854));
#6882=CARTESIAN_POINT('Ctrl Pts',(5.86345856579531,1.94180388956307,3.42941819783743));
#6883=CARTESIAN_POINT('Ctrl Pts',(5.85954884918067,1.93413605902323,3.36111065621248));
#6884=CARTESIAN_POINT('Ctrl Pts',(5.85563913256604,1.92286366321745,3.29324436238415));
#6885=CARTESIAN_POINT('Ctrl Pts',(5.85172941595141,1.90806947589925,3.22622125552985));
#6886=CARTESIAN_POINT('Ctrl Pts',(5.84781734878636,1.8932663942067,3.15915785389015));
#6887=CARTESIAN_POINT('Ctrl Pts',(5.8439052816213,1.87493743823196,3.09293912189533));
#6888=CARTESIAN_POINT('Ctrl Pts',(5.83999321445625,1.85321543256454,3.02795233175729));
#6889=CARTESIAN_POINT('Ctrl Pts',(5.83607441223039,1.83145603003688,2.96285365959759));
#6890=CARTESIAN_POINT('Ctrl Pts',(5.83215561000453,1.80629209935244,2.89899161930871));
#6891=CARTESIAN_POINT('Ctrl Pts',(5.82823680777867,1.77790445793083,2.83673317127403));
#6892=CARTESIAN_POINT('Ctrl Pts',(5.82642694385327,1.76479387842842,2.80797966123306));
#6893=CARTESIAN_POINT('Ctrl Pts',(5.82461707992786,1.75099633135706,2.77956783987747));
#6894=CARTESIAN_POINT('Ctrl Pts',(5.82280721600245,1.73653280861797,2.75153186464793));
#6895=CARTESIAN_POINT('Ctrl Pts',(5.81888944803674,1.70522397635551,2.69084307799401));
#6896=CARTESIAN_POINT('Ctrl Pts',(5.81497168007103,1.67066771919405,2.63167709240386));
#6897=CARTESIAN_POINT('Ctrl Pts',(5.81105391210533,1.63303593841818,2.57440349728987));
#6898=CARTESIAN_POINT('Ctrl Pts',(5.80714204705379,1.59546085757295,2.51721619649423));
#6899=CARTESIAN_POINT('Ctrl Pts',(5.80323018200225,1.55481971769912,2.46191603529415));
#6900=CARTESIAN_POINT('Ctrl Pts',(5.79931831695071,1.51133052729582,2.408848531605));
#6901=CARTESIAN_POINT('Ctrl Pts',(5.7954110563828,1.46789252609836,2.35584349133134));
#6902=CARTESIAN_POINT('Ctrl Pts',(5.79150379581489,1.42161344246653,2.30506626812452));
#6903=CARTESIAN_POINT('Ctrl Pts',(5.78759653524698,1.37275379361172,2.25683234377284));
#6904=CARTESIAN_POINT('Ctrl Pts',(5.78369172549626,1.32392479182156,2.20862867400204));
#6905=CARTESIAN_POINT('Ctrl Pts',(5.77978691574554,1.27251878501437,2.16296548343143));
#6906=CARTESIAN_POINT('Ctrl Pts',(5.77588210599482,1.21883461745178,2.12012298773394));
#6907=CARTESIAN_POINT('Ctrl Pts',(5.77197840559194,1.1651657014428,2.07729266349499));
#6908=CARTESIAN_POINT('Ctrl Pts',(5.76807470518906,1.10922029387594,2.03728175003941));
#6909=CARTESIAN_POINT('Ctrl Pts',(5.76417100478618,1.05133054742943,2.00033038937202));
#6910=CARTESIAN_POINT('Ctrl Pts',(5.76026707390628,0.993437383134513,1.96337684707219));
#6911=CARTESIAN_POINT('Ctrl Pts',(5.75636314302638,0.933600068134951,1.9294834787164));
#6912=CARTESIAN_POINT('Ctrl Pts',(5.75245921214648,0.872178434039021,1.89884627644092));
#6913=CARTESIAN_POINT('Ctrl Pts',(5.74855112949317,0.810691478933375,1.86817649194883));
#6914=CARTESIAN_POINT('Ctrl Pts',(5.74464304683987,0.747617283319029,1.84077000432081));
#6915=CARTESIAN_POINT('Ctrl Pts',(5.74073496418656,0.683337987343999,1.81677566715332));
#6916=CARTESIAN_POINT('Ctrl Pts',(5.73682454138663,0.619020201144718,1.79276696225818));
#6917=CARTESIAN_POINT('Ctrl Pts',(5.73291411858669,0.553496347862577,1.77217462161367));
#6918=CARTESIAN_POINT('Ctrl Pts',(5.72900369578676,0.487163454161308,1.75509751248396));
#6919=CARTESIAN_POINT('Ctrl Pts',(5.72508653679808,0.420716293815509,1.73799098591367));
#6920=CARTESIAN_POINT('Ctrl Pts',(5.7211693778094,0.353457793522223,1.72441187359348));
#6921=CARTESIAN_POINT('Ctrl Pts',(5.71725221882072,0.285794006257841,1.71440771561662));
#6922=CARTESIAN_POINT('Ctrl Pts',(5.71542803769094,0.254283668215885,1.70974888092201));
#6923=CARTESIAN_POINT('Ctrl Pts',(5.71360385656115,0.222685489647637,1.70586459717762));
#6924=CARTESIAN_POINT('Ctrl Pts',(5.71177967543137,0.191040535300942,1.70275580933668));
#6925=CARTESIAN_POINT('Ctrl Pts',(5.70786098451082,0.123061104281254,1.69607753683001));
#6926=CARTESIAN_POINT('Ctrl Pts',(5.70394229359028,0.0545967376770631,1.69295492978579));
#6927=CARTESIAN_POINT('Ctrl Pts',(5.70002360266973,-0.0139486777057676,
1.69344425540989));
#6928=CARTESIAN_POINT('Ctrl Pts',(5.69611080172421,-0.0823910661356112,
1.69393284555479));
#6929=CARTESIAN_POINT('Ctrl Pts',(5.6921980007787,-0.150913773809251,1.69802259030234));
#6930=CARTESIAN_POINT('Ctrl Pts',(5.68828519983318,-0.219108106246357,1.70571796644915));
#6931=CARTESIAN_POINT('Ctrl Pts',(5.68437698884756,-0.287222442472266,1.71340431543909));
#6932=CARTESIAN_POINT('Ctrl Pts',(5.68046877786194,-0.355008682184551,1.72468784075306));
#6933=CARTESIAN_POINT('Ctrl Pts',(5.67656056687632,-0.422060281410876,1.7395210136608));
#6934=CARTESIAN_POINT('Ctrl Pts',(5.67265479824836,-0.489069978092083,1.75434491687618));
#6935=CARTESIAN_POINT('Ctrl Pts',(5.6687490296204,-0.55534546597675,1.77271396128292));
#6936=CARTESIAN_POINT('Ctrl Pts',(5.66484326099244,-0.620489011696215,1.7945292852864));
#6937=CARTESIAN_POINT('Ctrl Pts',(5.66093859471864,-0.685614171467829,1.81633845218859));
#6938=CARTESIAN_POINT('Ctrl Pts',(5.65703392844483,-0.749607557261707,1.84159181166358));
#6939=CARTESIAN_POINT('Ctrl Pts',(5.65312926217103,-0.81208700473629,1.87014077318617));
#6940=CARTESIAN_POINT('Ctrl Pts',(5.64922435988424,-0.874570228707953,1.89869146031732));
#6941=CARTESIAN_POINT('Ctrl Pts',(5.64531945759746,-0.935538886526247,1.93053793828032));
#6942=CARTESIAN_POINT('Ctrl Pts',(5.64141455531067,-0.994632859047944,1.96548440062207));
#6943=CARTESIAN_POINT('Ctrl Pts',(5.63750549952043,-1.05378968769269,2.00046803425293));
#6944=CARTESIAN_POINT('Ctrl Pts',(5.6335964437302,-1.1110674275645,2.03855798189316));
#6945=CARTESIAN_POINT('Ctrl Pts',(5.62968738793996,-1.16613342782463,2.07951410661402));
#6946=CARTESIAN_POINT('Ctrl Pts',(5.62577598959698,-1.22123242710478,2.12049477482766));
#6947=CARTESIAN_POINT('Ctrl Pts',(5.621864591254,-1.2741166703757,2.16434472458644));
#6948=CARTESIAN_POINT('Ctrl Pts',(5.61795319291102,-1.32448739361131,2.21078417172996));
#6949=CARTESIAN_POINT('Ctrl Pts',(5.61403506488184,-1.37494478129035,2.25730351943042));
#6950=CARTESIAN_POINT('Ctrl Pts',(5.61011693685267,-1.42287967463459,2.30642090478235));
#6951=CARTESIAN_POINT('Ctrl Pts',(5.6061988088235,-1.46803150387178,2.3578210878049));
#6952=CARTESIAN_POINT('Ctrl Pts',(5.60438325083577,-1.48895367987577,2.38163858742791));
#6953=CARTESIAN_POINT('Ctrl Pts',(5.60256769284803,-1.50927887683695,2.40594579641597));
#6954=CARTESIAN_POINT('Ctrl Pts',(5.60075213486029,-1.52898432404688,2.43070924324869));
#6955=CARTESIAN_POINT('Ctrl Pts',(5.59684165166294,-1.57142737501594,2.48404658824237));
#6956=CARTESIAN_POINT('Ctrl Pts',(5.59293116846558,-1.6111640527522,2.53971800749396));
#6957=CARTESIAN_POINT('Ctrl Pts',(5.58902068526823,-1.64792721276267,2.59741737261166));
#6958=CARTESIAN_POINT('Ctrl Pts',(5.58511589987983,-1.68463680664033,2.65503266628787));
#6959=CARTESIAN_POINT('Ctrl Pts',(5.58121111449144,-1.71838121312398,2.71466963328178));
#6960=CARTESIAN_POINT('Ctrl Pts',(5.57730632910304,-1.7489338680892,2.77598966852054));
#6961=CARTESIAN_POINT('Ctrl Pts',(5.57340588306939,-1.77945257014912,2.8372415593263));
#6962=CARTESIAN_POINT('Ctrl Pts',(5.56950543703574,-1.80678633979231,2.9001723678975));
#6963=CARTESIAN_POINT('Ctrl Pts',(5.5656049910021,-1.83075322221421,2.96441669459553));
#6964=CARTESIAN_POINT('Ctrl Pts',(5.56170723775053,-1.85470355842809,3.02861666842466));
#6965=CARTESIAN_POINT('Ctrl Pts',(5.55780948449896,-1.87529144678611,3.09412790017198));
#6966=CARTESIAN_POINT('Ctrl Pts',(5.5539117312474,-1.89238272508188,3.16056429069452));
#6967=CARTESIAN_POINT('Ctrl Pts',(5.55001553362784,-1.90946718207883,3.22697416579414));
#6968=CARTESIAN_POINT('Ctrl Pts',(5.54611933600829,-1.92305768028661,3.29430798817087));
#6969=CARTESIAN_POINT('Ctrl Pts',(5.54222313838873,-1.93307022193267,3.36216558286517));
#6970=CARTESIAN_POINT('Ctrl Pts',(5.53832611196746,-1.94308489345316,3.4300376122716));
#6971=CARTESIAN_POINT('Ctrl Pts',(5.53442908554619,-1.94952001575366,3.49843314824966));
#6972=CARTESIAN_POINT('Ctrl Pts',(5.53053205912492,-1.9523431543508,3.56694443621705));
#6973=CARTESIAN_POINT('Ctrl Pts',(5.52897793679136,-1.95346901347268,3.59426653035276));
#6974=CARTESIAN_POINT('Ctrl Pts',(5.52742381445779,-1.95402100669827,3.62160699243968));
#6975=CARTESIAN_POINT('Ctrl Pts',(5.52586969212423,-1.95399938885048,3.64893990412505));
#6976=CARTESIAN_POINT('Ctrl Pts',(5.42413030787577,-1.95399943981962,3.64887405762318));
#6977=CARTESIAN_POINT('Ctrl Pts',(5.42803486416928,-1.9540514551376,3.58018073880961));
#6978=CARTESIAN_POINT('Ctrl Pts',(5.4319394204628,-1.95047675797587,3.51144725141454));
#6979=CARTESIAN_POINT('Ctrl Pts',(5.43584397675631,-1.94328925495971,3.4430837452218));
#6980=CARTESIAN_POINT('Ctrl Pts',(5.43974798134642,-1.93610276751858,3.37472989861042));
#6981=CARTESIAN_POINT('Ctrl Pts',(5.44365198593652,-1.92530453973603,3.30674641766514));
#6982=CARTESIAN_POINT('Ctrl Pts',(5.44755599052663,-1.91096035466862,3.23953846074591));
#6983=CARTESIAN_POINT('Ctrl Pts',(5.45146077678909,-1.89661329756235,3.17231704723347));
#6984=CARTESIAN_POINT('Ctrl Pts',(5.45536556305155,-1.87871897897925,3.10587194559481));
#6985=CARTESIAN_POINT('Ctrl Pts',(5.45927034931401,-1.85739392663885,3.04059647777541));
#6986=CARTESIAN_POINT('Ctrl Pts',(5.46317986564956,-1.8360430421403,2.97524193834664));
#6987=CARTESIAN_POINT('Ctrl Pts',(5.46708938198511,-1.81125328691819,2.91106032641271));
#6988=CARTESIAN_POINT('Ctrl Pts',(5.47099889832066,-1.78319022584853,2.8484272484067));
#6989=CARTESIAN_POINT('Ctrl Pts',(5.4749112282153,-1.75510696865389,2.78574909529402));
#6990=CARTESIAN_POINT('Ctrl Pts',(5.47882355810994,-1.7237459439217,2.72462212920013));
#6991=CARTESIAN_POINT('Ctrl Pts',(5.48273588800458,-1.68931847990927,2.66539697672035));
#6992=CARTESIAN_POINT('Ctrl Pts',(5.48665507658779,-1.65483066125905,2.60606799688273));
#6993=CARTESIAN_POINT('Ctrl Pts',(5.49057426517099,-1.61726594887423,2.54864789067703));
#6994=CARTESIAN_POINT('Ctrl Pts',(5.49449345375419,-1.57687814704107,2.4934571608948));
#6995=CARTESIAN_POINT('Ctrl Pts',(5.49557683430917,-1.56571375465847,2.47820079795344));
#6996=CARTESIAN_POINT('Ctrl Pts',(5.49666021486415,-1.55433386759309,2.4631145830252));
#6997=CARTESIAN_POINT('Ctrl Pts',(5.49774359541912,-1.54274435158162,2.44820479785512));
#6998=CARTESIAN_POINT('Ctrl Pts',(5.5016621214048,-1.50082572987125,2.39427695102282));
#6999=CARTESIAN_POINT('Ctrl Pts',(5.50558064739048,-1.4559931807208,2.3424430626892));
#7000=CARTESIAN_POINT('Ctrl Pts',(5.50949917337616,-1.40848368839704,2.29303495193695));
#7001=CARTESIAN_POINT('Ctrl Pts',(5.51341180805355,-1.36104562422436,2.24370112381384));
#7002=CARTESIAN_POINT('Ctrl Pts',(5.51732444273093,-1.31093894257672,2.19678618675945));
#7003=CARTESIAN_POINT('Ctrl Pts',(5.52123707740832,-1.25844152415246,2.15258982208797));
#7004=CARTESIAN_POINT('Ctrl Pts',(5.52514512098626,-1.20600570638572,2.10844531758802));
#7005=CARTESIAN_POINT('Ctrl Pts',(5.5290531645642,-1.15118509767119,2.06701336528421));
#7006=CARTESIAN_POINT('Ctrl Pts',(5.53296120814214,-1.09429384419977,2.02855631005233));
#7007=CARTESIAN_POINT('Ctrl Pts',(5.53686680875612,-1.03743815411925,1.99012329477747));
#7008=CARTESIAN_POINT('Ctrl Pts',(5.54077240937011,-0.978514793457697,1.95466176237219));
#7009=CARTESIAN_POINT('Ctrl Pts',(5.5446780099841,-0.917869103633582,1.92239234985187));
#7010=CARTESIAN_POINT('Ctrl Pts',(5.54858250789829,-0.857240536397237,1.89013204821561));
#7011=CARTESIAN_POINT('Ctrl Pts',(5.55248700581249,-0.794891039285522,1.86106230817238));
#7012=CARTESIAN_POINT('Ctrl Pts',(5.55639150372669,-0.731191334976379,1.83535825682024));
#7013=CARTESIAN_POINT('Ctrl Pts',(5.56029623756837,-0.667487781642105,1.8096526523127));
#7014=CARTESIAN_POINT('Ctrl Pts',(5.56420097141004,-0.602434316123581,1.78731332188342));
#7015=CARTESIAN_POINT('Ctrl Pts',(5.56810570525172,-0.536420762695307,1.7684669110456));
#7016=CARTESIAN_POINT('Ctrl Pts',(5.57201459363006,-0.470336972539247,1.74960044811));
#7017=CARTESIAN_POINT('Ctrl Pts',(5.5759234820084,-0.403291529645279,1.73423445667239));
#7018=CARTESIAN_POINT('Ctrl Pts',(5.57983237038674,-0.335687534543338,1.72244514969072));
#7019=CARTESIAN_POINT('Ctrl Pts',(5.58374360166571,-0.26804301911242,1.71064877646102));
#7020=CARTESIAN_POINT('Ctrl Pts',(5.58765483294468,-0.199839773474244,1.70243341304379));
#7021=CARTESIAN_POINT('Ctrl Pts',(5.59156606422366,-0.131486358979629,1.69782340330515));
#7022=CARTESIAN_POINT('Ctrl Pts',(5.59548402748142,-0.0630152951557196,
1.69320545885603));
#7023=CARTESIAN_POINT('Ctrl Pts',(5.59940199073919,0.00560596196072642,
1.69220526025078));
#7024=CARTESIAN_POINT('Ctrl Pts',(5.60331995399695,0.0739693956149147,1.69479503969838));
#7025=CARTESIAN_POINT('Ctrl Pts',(5.60513701466137,0.10567477364043,1.69599611945697));
#7026=CARTESIAN_POINT('Ctrl Pts',(5.60695407532578,0.137324779937523,1.69796863240155));
#7027=CARTESIAN_POINT('Ctrl Pts',(5.6087711359902,0.168879356249839,1.70070605895056));
#7028=CARTESIAN_POINT('Ctrl Pts',(5.6126895205751,0.236924946485997,1.70660915850138));
#7029=CARTESIAN_POINT('Ctrl Pts',(5.61660790515999,0.304795263666359,1.71609598339351));
#7030=CARTESIAN_POINT('Ctrl Pts',(5.62052628974489,0.372083006075865,1.72914781141475));
#7031=CARTESIAN_POINT('Ctrl Pts',(5.62443878264703,0.43926957464105,1.74218001470839));
#7032=CARTESIAN_POINT('Ctrl Pts',(5.62835127554917,0.505874827988566,1.75876648978475));
#7033=CARTESIAN_POINT('Ctrl Pts',(5.6322637684513,0.571496231559635,1.77883672036353));
#7034=CARTESIAN_POINT('Ctrl Pts',(5.63617167038825,0.637040634203925,1.79888340029768));
#7035=CARTESIAN_POINT('Ctrl Pts',(5.6400795723252,0.701603011786189,1.82240557394214));
#7036=CARTESIAN_POINT('Ctrl Pts',(5.64398747426214,0.764792477692673,1.84928199514302));
#7037=CARTESIAN_POINT('Ctrl Pts',(5.64789293340082,0.827942444368987,1.87614161610779));
#7038=CARTESIAN_POINT('Ctrl Pts',(5.6517983925395,0.889720750222788,1.90635113331972));
#7039=CARTESIAN_POINT('Ctrl Pts',(5.65570385167817,0.949754581589691,1.93974045334133));
#7040=CARTESIAN_POINT('Ctrl Pts',(5.65960820849432,1.00977146830488,1.97312034917018));
#7041=CARTESIAN_POINT('Ctrl Pts',(5.66351256531046,1.06804442841491,2.00967802715195));
#7042=CARTESIAN_POINT('Ctrl Pts',(5.66741692212661,1.12422507203647,2.04919736297908));
#7043=CARTESIAN_POINT('Ctrl Pts',(5.67132151545936,1.18040911894727,2.08871909279322));
#7044=CARTESIAN_POINT('Ctrl Pts',(5.67522610879212,1.23450019697237,2.1312025515863));
#7045=CARTESIAN_POINT('Ctrl Pts',(5.67913070212488,1.28618024652914,2.17638924278729));
#7046=CARTESIAN_POINT('Ctrl Pts',(5.68303945183553,1.33791530868184,2.22162403450687));
#7047=CARTESIAN_POINT('Ctrl Pts',(5.68694820154618,1.38723384954996,2.26956747692691));
#7048=CARTESIAN_POINT('Ctrl Pts',(5.69085695125683,1.43385294230903,2.31992253267402));
#7049=CARTESIAN_POINT('Ctrl Pts',(5.69476804471798,1.48049998864158,2.37030778213938));
#7050=CARTESIAN_POINT('Ctrl Pts',(5.69867913817914,1.52444405084874,2.42310714477378));
#7051=CARTESIAN_POINT('Ctrl Pts',(5.70259023164029,1.56544278674034,2.47799082477893));
#7052=CARTESIAN_POINT('Ctrl Pts',(5.70650805982365,1.60651212056052,2.53296901194476));
#7053=CARTESIAN_POINT('Ctrl Pts',(5.710425888007,1.64462573292583,2.59003827089));
#7054=CARTESIAN_POINT('Ctrl Pts',(5.71434371619036,1.67958533188226,2.64884095798712));
#7055=CARTESIAN_POINT('Ctrl Pts',(5.716162036314,1.69581058202645,2.67613212652971));
#7056=CARTESIAN_POINT('Ctrl Pts',(5.71798035643764,1.71135711117411,2.7037963513432));
#7057=CARTESIAN_POINT('Ctrl Pts',(5.71979867656128,1.72620860178437,2.73179637789395));
#7058=CARTESIAN_POINT('Ctrl Pts',(5.7237172632497,1.75821443653913,2.79213808004565));
#7059=CARTESIAN_POINT('Ctrl Pts',(5.72763584993812,1.78711577385686,2.85427932151725));
#7060=CARTESIAN_POINT('Ctrl Pts',(5.73155443662654,1.81270709470793,2.91786791715942));
#7061=CARTESIAN_POINT('Ctrl Pts',(5.73546713106489,1.83825993473059,2.9813608967194));
#7062=CARTESIAN_POINT('Ctrl Pts',(5.73937982550325,1.86051245417103,3.04629645861379));
#7063=CARTESIAN_POINT('Ctrl Pts',(5.7432925199416,1.87930521175744,3.11229828902138));
#7064=CARTESIAN_POINT('Ctrl Pts',(5.74720062162182,1.89807591022535,3.1782226458495));
#7065=CARTESIAN_POINT('Ctrl Pts',(5.75110872330204,1.91339477829522,3.24521031476398));
#7066=CARTESIAN_POINT('Ctrl Pts',(5.75501682498226,1.925151295957,3.31286720829584));
#7067=CARTESIAN_POINT('Ctrl Pts',(5.7589224826383,1.93690046140132,3.38048179098295));
#7068=CARTESIAN_POINT('Ctrl Pts',(5.76282814029434,1.94509161174389,3.4487642846754));
#7069=CARTESIAN_POINT('Ctrl Pts',(5.76673379795039,1.94966505701592,3.5173092444838));
#7070=CARTESIAN_POINT('Ctrl Pts',(5.77063835177014,1.95423720971821,3.58583483177652));
#7071=CARTESIAN_POINT('Ctrl Pts',(5.77454290558989,1.95519365441088,3.65462224750219));
#7072=CARTESIAN_POINT('Ctrl Pts',(5.77844745940964,1.9525266159011,3.72326155072272));
#7073=CARTESIAN_POINT('Ctrl Pts',(5.7823522479429,1.94985941706828,3.79190498004124));
#7074=CARTESIAN_POINT('Ctrl Pts',(5.78625703647617,1.94356832425448,3.86039978791119));
#7075=CARTESIAN_POINT('Ctrl Pts',(5.79016182500943,1.93369761352097,3.92833848310408));
#7076=CARTESIAN_POINT('Ctrl Pts',(5.79407076589633,1.92381640626984,3.99634942433178));
#7077=CARTESIAN_POINT('Ctrl Pts',(5.79797970678323,1.91034805528966,4.06380258514446));
#7078=CARTESIAN_POINT('Ctrl Pts',(5.80188864767013,1.8933882795822,4.13029903726282));
#7079=CARTESIAN_POINT('Ctrl Pts',(5.80579993028798,1.8764183437744,4.19683532544022));
#7080=CARTESIAN_POINT('Ctrl Pts',(5.80971121290583,1.85595296703639,4.26241329480045));
#7081=CARTESIAN_POINT('Ctrl Pts',(5.81362249552368,1.83213741818903,4.32665029701972));
#7082=CARTESIAN_POINT('Ctrl Pts',(5.81754050780242,1.80828089286843,4.39099782391425));
#7083=CARTESIAN_POINT('Ctrl Pts',(5.82145852008116,1.78106288604147,4.45399932770491));
#7084=CARTESIAN_POINT('Ctrl Pts',(5.82537653235989,1.75067597596596,4.51529401729611));
#7085=CARTESIAN_POINT('Ctrl Pts',(5.82719309395072,1.73658727746786,4.54371291211097));
#7086=CARTESIAN_POINT('Ctrl Pts',(5.82900965554154,1.7218180070699,4.5717652764579));
#7087=CARTESIAN_POINT('Ctrl Pts',(5.83082621713236,1.70639051229435,4.59941727239722));
#7088=CARTESIAN_POINT('Ctrl Pts',(5.8347449049416,1.67311031083597,4.65906817547481));
#7089=CARTESIAN_POINT('Ctrl Pts',(5.83866359275085,1.63663272637616,4.7170897663396));
#7090=CARTESIAN_POINT('Ctrl Pts',(5.84258228056009,1.59714186055191,4.7731181809562));
#7091=CARTESIAN_POINT('Ctrl Pts',(5.84649507869295,1.55771034837637,4.82906238645838));
#7092=CARTESIAN_POINT('Ctrl Pts',(5.85040787682581,1.51527482417692,4.88301896247133));
#7093=CARTESIAN_POINT('Ctrl Pts',(5.85432067495868,1.47006467497947,4.93464963000493));
#7094=CARTESIAN_POINT('Ctrl Pts',(5.85822888358509,1.42490755490964,4.98621973748052));
#7095=CARTESIAN_POINT('Ctrl Pts',(5.8621370922115,1.37698259577563,5.03546898652637));
#7096=CARTESIAN_POINT('Ctrl Pts',(5.86604530083791,1.32656067870888,5.08209052170544));
#7097=CARTESIAN_POINT('Ctrl Pts',(5.86995106738939,1.27617026817394,5.12868292505125));
#7098=CARTESIAN_POINT('Ctrl Pts',(5.87385683394088,1.2232863550066,5.17265053860784));
#7099=CARTESIAN_POINT('Ctrl Pts',(5.87776260049236,1.16821696380866,5.21372301794058));
#7100=CARTESIAN_POINT('Ctrl Pts',(5.88166726497468,1.11316311124502,5.25478390807245));
#7101=CARTESIAN_POINT('Ctrl Pts',(5.88557192945699,1.05592539883243,5.29295099187428));
#7102=CARTESIAN_POINT('Ctrl Pts',(5.88947659393931,0.996843822961791,5.32799507301508));
#7103=CARTESIAN_POINT('Ctrl Pts',(5.89338149472209,0.937758671622883,5.36304127493548));
#7104=CARTESIAN_POINT('Ctrl Pts',(5.89728639550488,0.876829859508901,5.39496385033934));
#7105=CARTESIAN_POINT('Ctrl Pts',(5.90119129628766,0.814423597314107,5.42357863782766));
#7106=CARTESIAN_POINT('Ctrl Pts',(5.90510035101687,0.751950948728358,5.4522238650892));
#7107=CARTESIAN_POINT('Ctrl Pts',(5.90900940574608,0.687998161327613,5.47755407684429));
#7108=CARTESIAN_POINT('Ctrl Pts',(5.91291846047529,0.62295219724466,5.49943295599088));
#7109=CARTESIAN_POINT('Ctrl Pts',(5.91682985800875,0.55786724932253,5.5213249477528));
#7110=CARTESIAN_POINT('Ctrl Pts',(5.92074125554221,0.491688294525717,5.53976135825004));
#7111=CARTESIAN_POINT('Ctrl Pts',(5.92465265307567,0.424815539002211,5.55465631654233));
#7112=CARTESIAN_POINT('Ctrl Pts',(5.92857078068969,0.35782771999363,5.56957690359475));
#7113=CARTESIAN_POINT('Ctrl Pts',(5.9324889083037,0.29014420234409,5.58094379549625));
#7114=CARTESIAN_POINT('Ctrl Pts',(5.93640703591772,0.222172536783606,5.58872271561845));
#7115=CARTESIAN_POINT('Ctrl Pts',(5.93822260984629,0.190675965964468,5.59232729565198));
#7116=CARTESIAN_POINT('Ctrl Pts',(5.94003818377486,0.159117552570715,5.59516220427779));
#7117=CARTESIAN_POINT('Ctrl Pts',(5.94185375770344,0.127537778503502,5.59722782399774));
#7118=CARTESIAN_POINT('Ctrl Pts',(5.94577148616542,0.0593934976570033,5.6016851127047));
#7119=CARTESIAN_POINT('Ctrl Pts',(5.94968921462741,-0.00911979872307073,
5.60257459642064));
#7120=CARTESIAN_POINT('Ctrl Pts',(5.9536069430894,-0.0775967852894685,5.59985310777223));
#7121=CARTESIAN_POINT('Ctrl Pts',(5.95751877860343,-0.145970770506587,5.59713571271813));
#7122=CARTESIAN_POINT('Ctrl Pts',(5.96143061411747,-0.214308066664483,5.59081814430949));
#7123=CARTESIAN_POINT('Ctrl Pts',(5.96534244963151,-0.282200215530251,5.58090915360557));
#7124=CARTESIAN_POINT('Ctrl Pts',(5.96924969548283,-0.350012708167429,5.5710117888826));
#7125=CARTESIAN_POINT('Ctrl Pts',(5.97315694133415,-0.417380606242612,5.55753144105242));
#7126=CARTESIAN_POINT('Ctrl Pts',(5.97706418718548,-0.483899283145357,5.54052876985136));
#7127=CARTESIAN_POINT('Ctrl Pts',(5.98096899142348,-0.550376392945782,5.52353672351245));
#7128=CARTESIAN_POINT('Ctrl Pts',(5.98487379566148,-0.616004858668716,5.50302684158917));
#7129=CARTESIAN_POINT('Ctrl Pts',(5.98877859989948,-0.680390524083188,5.47911080405691));
#7130=CARTESIAN_POINT('Ctrl Pts',(5.99268230397228,-0.744758049057379,5.45520150478615));
#7131=CARTESIAN_POINT('Ctrl Pts',(5.99658600804508,-0.807883007867782,5.42788812625633));
#7132=CARTESIAN_POINT('Ctrl Pts',(6.00048971211789,-0.869388420973091,5.39733154528919));
#7133=CARTESIAN_POINT('Ctrl Pts',(6.00439365583889,-0.930897609892601,5.36677308845508));
#7134=CARTESIAN_POINT('Ctrl Pts',(6.00829759955989,-0.990786616270124,5.3329712551077));
#7135=CARTESIAN_POINT('Ctrl Pts',(6.01220154328089,-1.04870203159526,5.29613339513917));
#7136=CARTESIAN_POINT('Ctrl Pts',(6.01610965249554,-1.10667924245652,5.25925622930892));
#7137=CARTESIAN_POINT('Ctrl Pts',(6.0200177617102,-1.16267824386887,5.21933683660942));
#7138=CARTESIAN_POINT('Ctrl Pts',(6.02392587092486,-1.21637452603557,5.17662597868762));
#7139=CARTESIAN_POINT('Ctrl Pts',(6.02783632816032,-1.27010306932417,5.13388945976774));
#7140=CARTESIAN_POINT('Ctrl Pts',(6.03174678539579,-1.32152577164834,5.08835846406956));
#7141=CARTESIAN_POINT('Ctrl Pts',(6.03565724263125,-1.37035328888209,5.04032227102529));
#7142=CARTESIAN_POINT('Ctrl Pts',(6.03957444778363,-1.41926506327798,4.99220318633436));
#7143=CARTESIAN_POINT('Ctrl Pts',(6.043491652936,-1.46557238303484,4.94157063931874));
#7144=CARTESIAN_POINT('Ctrl Pts',(6.04740885808838,-1.50902523794519,4.88874809688632));
#7145=CARTESIAN_POINT('Ctrl Pts',(6.04923300481709,-1.52926017077472,4.86414992951135));
#7146=CARTESIAN_POINT('Ctrl Pts',(6.0510571515458,-1.54887670810727,4.83907727941775));
#7147=CARTESIAN_POINT('Ctrl Pts',(6.05288129827451,-1.56785287850625,4.81356484664188));
#7148=CARTESIAN_POINT('Ctrl Pts',(6.05681837522051,-1.6088093661754,4.75850106841764));
#7149=CARTESIAN_POINT('Ctrl Pts',(6.06075545216651,-1.64694295803685,4.70116771866654));
#7150=CARTESIAN_POINT('Ctrl Pts',(6.06469252911251,-1.68199473772209,4.64188413754907));
#7151=CARTESIAN_POINT('Ctrl Pts',(6.06862362532713,-1.71699327098078,4.58269061288167));
#7152=CARTESIAN_POINT('Ctrl Pts',(6.07255472154176,-1.74891903684483,4.52155314947086));
#7153=CARTESIAN_POINT('Ctrl Pts',(6.07648581775639,-1.7775548481719,4.45882207549266));
#7154=CARTESIAN_POINT('Ctrl Pts',(6.080456191933,-1.80647677722476,4.39546421737978));
#7155=CARTESIAN_POINT('Ctrl Pts',(6.08442656610961,-1.83204232976782,4.33048112322188));
#7156=CARTESIAN_POINT('Ctrl Pts',(6.08839694028623,-1.85407425987925,4.26426126010623));
#7157=CARTESIAN_POINT('Ctrl Pts',(6.09231991040319,-1.87584314099758,4.1988320253299));
#7158=CARTESIAN_POINT('Ctrl Pts',(6.09624288052014,-1.89416217128946,4.13219586906046));
#7159=CARTESIAN_POINT('Ctrl Pts',(6.1001658506371,-1.9089086849858,4.06474759500726));
#7160=CARTESIAN_POINT('Ctrl Pts',(6.10415992684354,-1.92392248772367,3.99607678219701));
#7161=CARTESIAN_POINT('Ctrl Pts',(6.10815400304999,-1.93523279654417,3.92656460262322));
#7162=CARTESIAN_POINT('Ctrl Pts',(6.11214807925643,-1.94276391462491,3.85664162365595));
#7163=CARTESIAN_POINT('Ctrl Pts',(6.11614215546288,-1.95029503270565,3.78671864468868));
#7164=CARTESIAN_POINT('Ctrl Pts',(6.12013623166933,-1.95404689998987,3.71638539512174));
#7165=CARTESIAN_POINT('Ctrl Pts',(6.12413030787577,-1.95399955699113,3.64607868772758));
#7166=CARTESIAN_POINT('Origin',(0.,0.,3.64739446828387));
#7167=CARTESIAN_POINT('',(6.59995882699137,0.834037993952276,5.41445321791391));
#7168=CARTESIAN_POINT('Ctrl Pts',(6.12413030792735,-1.95399955699052,3.6460786868197));
#7169=CARTESIAN_POINT('Ctrl Pts',(6.128579472032,-1.95394681966027,3.56776118292618));
#7170=CARTESIAN_POINT('Ctrl Pts',(6.13302863613666,-1.9491815174852,3.48962762197139));
#7171=CARTESIAN_POINT('Ctrl Pts',(6.13747780024132,-1.93979384649703,3.41220128578861));
#7172=CARTESIAN_POINT('Ctrl Pts',(6.14196527052808,-1.93032535002662,3.33410832835666));
#7173=CARTESIAN_POINT('Ctrl Pts',(6.14645274081484,-1.91615465962242,3.25673503473373));
#7174=CARTESIAN_POINT('Ctrl Pts',(6.1509402111016,-1.89742413111203,3.18059936690237));
#7175=CARTESIAN_POINT('Ctrl Pts',(6.15526308701627,-1.87938061318493,3.10725625292429));
#7176=CARTESIAN_POINT('Ctrl Pts',(6.15958596293093,-1.85710603049991,3.03506166685608));
#7177=CARTESIAN_POINT('Ctrl Pts',(6.1639088388456,-1.83076925289313,2.96445966710507));
#7178=CARTESIAN_POINT('Ctrl Pts',(6.16782834248828,-1.80688998876341,2.90044561704503));
#7179=CARTESIAN_POINT('Ctrl Pts',(6.17174784613096,-1.7796022508274,2.83755952478642));
#7180=CARTESIAN_POINT('Ctrl Pts',(6.17566734977364,-1.74903318078112,2.77618902034024));
#7181=CARTESIAN_POINT('Ctrl Pts',(6.17958097555391,-1.71850995347519,2.7149105498387));
#7182=CARTESIAN_POINT('Ctrl Pts',(6.18349460133418,-1.68471537782724,2.65514359264594));
#7183=CARTESIAN_POINT('Ctrl Pts',(6.18740822711445,-1.64782522231827,2.59725731691185));
#7184=CARTESIAN_POINT('Ctrl Pts',(6.19131727661406,-1.61097820320371,2.5394387287542));
#7185=CARTESIAN_POINT('Ctrl Pts',(6.19522632611367,-1.5710430561003,2.48349686699584));
#7186=CARTESIAN_POINT('Ctrl Pts',(6.19913537561328,-1.52824131094062,2.42977609804857));
#7187=CARTESIAN_POINT('Ctrl Pts',(6.2030419907236,-1.48546622088209,2.37608878410468));
#7188=CARTESIAN_POINT('Ctrl Pts',(6.20694860583392,-1.43982837971601,2.32462020257689));
#7189=CARTESIAN_POINT('Ctrl Pts',(6.21085522094425,-1.39159154689863,2.27568423408706));
#7190=CARTESIAN_POINT('Ctrl Pts',(6.21476074031502,-1.34336824369806,2.22676199130979));
#7191=CARTESIAN_POINT('Ctrl Pts',(6.21866625968579,-1.29254774089066,2.18037130118336));
#7192=CARTESIAN_POINT('Ctrl Pts',(6.22257177905657,-1.23943161720214,2.13679019638481));
#7193=CARTESIAN_POINT('Ctrl Pts',(6.22647753970867,-1.1863122120221,2.09320639916415));
#7194=CARTESIAN_POINT('Ctrl Pts',(6.23038330036077,-1.13089728596084,2.05243284162797));
#7195=CARTESIAN_POINT('Ctrl Pts',(6.23428906101287,-1.07352113506549,2.01470699893534));
#7196=CARTESIAN_POINT('Ctrl Pts',(6.23819897711688,-1.01608394002089,1.97694101862568));
#7197=CARTESIAN_POINT('Ctrl Pts',(6.2421088932209,-0.956681767401127,1.94222949473819));
#7198=CARTESIAN_POINT('Ctrl Pts',(6.24601880932491,-0.895676657146052,1.91076574404726));
#7199=CARTESIAN_POINT('Ctrl Pts',(6.24993107033161,-0.834634960160559,1.87928312353117));
#7200=CARTESIAN_POINT('Ctrl Pts',(6.2538433313383,-0.771988860386667,1.8510523547138));
#7201=CARTESIAN_POINT('Ctrl Pts',(6.257755592345,-0.708121117161733,1.82621889096311));
#7202=CARTESIAN_POINT('Ctrl Pts',(6.26167457751989,-0.644143601749422,1.80134274488956));
#7203=CARTESIAN_POINT('Ctrl Pts',(6.26559356269479,-0.578940718830281,1.77987571125724));
#7204=CARTESIAN_POINT('Ctrl Pts',(6.26951254786969,-0.512910290448902,1.76191335356762));
#7205=CARTESIAN_POINT('Ctrl Pts',(6.27132049171868,-0.482448499574295,1.75362678634447));
#7206=CARTESIAN_POINT('Ctrl Pts',(6.27312843556768,-0.45181072436177,1.74608538440029));
#7207=CARTESIAN_POINT('Ctrl Pts',(6.27493637941667,-0.421036523795824,1.73929482580449));
#7208=CARTESIAN_POINT('Ctrl Pts',(6.27884955238992,-0.354427834596099,1.72459711802713));
#7209=CARTESIAN_POINT('Ctrl Pts',(6.28276272536317,-0.286914720102418,1.71336187894293));
#7210=CARTESIAN_POINT('Ctrl Pts',(6.28667589833642,-0.218890401956766,1.70569341201099));
#7211=CARTESIAN_POINT('Ctrl Pts',(6.29058316674399,-0.150968725339424,1.69803651598762));
#7212=CARTESIAN_POINT('Ctrl Pts',(6.29449043515156,-0.0825378619267242,
1.69393576663677));
#7213=CARTESIAN_POINT('Ctrl Pts',(6.29839770355913,-0.0140020575316097,
1.693444637202));
#7214=CARTESIAN_POINT('Ctrl Pts',(6.30230038694881,0.0544533229314145,1.6929540840873));
#7215=CARTESIAN_POINT('Ctrl Pts',(6.3062030703385,0.123012908974606,1.69606474292709));
#7216=CARTESIAN_POINT('Ctrl Pts',(6.31010575372818,0.191268328644095,1.70277820113559));
#7217=CARTESIAN_POINT('Ctrl Pts',(6.31400600085657,0.259481139672197,1.70948746844857));
#7218=CARTESIAN_POINT('Ctrl Pts',(6.31790624798496,0.327389671181229,1.7197950259574));
#7219=CARTESIAN_POINT('Ctrl Pts',(6.32180649511335,0.394588140713679,1.7336504417202));
#7220=CARTESIAN_POINT('Ctrl Pts',(6.3257056540783,0.461767861968184,1.7475019918416));
#7221=CARTESIAN_POINT('Ctrl Pts',(6.32960481304326,0.528237431631385,1.76489933579883));
#7222=CARTESIAN_POINT('Ctrl Pts',(6.33350397200822,0.593600579199207,1.78574080759014));
#7223=CARTESIAN_POINT('Ctrl Pts',(6.33740338928221,0.65896805690377,1.80658366007418));
#7224=CARTESIAN_POINT('Ctrl Pts',(6.3413028065562,0.723228497863452,1.83087094102834));
#7225=CARTESIAN_POINT('Ctrl Pts',(6.34520222383019,0.786001893430872,1.85845147771008));
#7226=CARTESIAN_POINT('Ctrl Pts',(6.34910586523305,0.848843289649043,1.88606189161013));
#7227=CARTESIAN_POINT('Ctrl Pts',(6.3530095066359,0.910193973351115,1.91697248177239));
#7228=CARTESIAN_POINT('Ctrl Pts',(6.35691314803876,0.969695934475873,1.9509847905642));
#7229=CARTESIAN_POINT('Ctrl Pts',(6.36081916424754,1.02923409401004,1.98501779096777));
#7230=CARTESIAN_POINT('Ctrl Pts',(6.36472518045632,1.08692087827308,2.02215599775593));
#7231=CARTESIAN_POINT('Ctrl Pts',(6.3686311966651,1.14242723508608,2.06215757351591));
#7232=CARTESIAN_POINT('Ctrl Pts',(6.37254404842718,1.19803072837793,2.10222915228889));
#7233=CARTESIAN_POINT('Ctrl Pts',(6.37645690018926,1.25144579487274,2.14517379158577));
#7234=CARTESIAN_POINT('Ctrl Pts',(6.38036975195135,1.30237711460555,2.1907099275024));
#7235=CARTESIAN_POINT('Ctrl Pts',(6.38223447463015,1.32664912712779,2.21241079186211));
#7236=CARTESIAN_POINT('Ctrl Pts',(6.38409919730895,1.35035760118791,2.23469968813216));
#7237=CARTESIAN_POINT('Ctrl Pts',(6.38596391998775,1.37347374173203,2.25754344001767));
#7238=CARTESIAN_POINT('Ctrl Pts',(6.38988983122375,1.42214152323476,2.30563774552445));
#7239=CARTESIAN_POINT('Ctrl Pts',(6.39381574245974,1.46837481356246,2.35638495257544));
#7240=CARTESIAN_POINT('Ctrl Pts',(6.39774165369574,1.5118716955992,2.40950918440414));
#7241=CARTESIAN_POINT('Ctrl Pts',(6.401661650329,1.55530304717378,2.46255338163494));
#7242=CARTESIAN_POINT('Ctrl Pts',(6.40558164696225,1.59600586540517,2.51796711955856));
#7243=CARTESIAN_POINT('Ctrl Pts',(6.40950164359551,1.63371504486074,2.57543777503752));
#7244=CARTESIAN_POINT('Ctrl Pts',(6.4134169792512,1.67137938712486,2.63284009641798));
#7245=CARTESIAN_POINT('Ctrl Pts',(6.41733231490688,1.70605689353566,2.69229406976241));
#7246=CARTESIAN_POINT('Ctrl Pts',(6.42124765056257,1.73752386585782,2.75345553548449));
#7247=CARTESIAN_POINT('Ctrl Pts',(6.42516049537214,1.76897081961895,2.81457809169465));
#7248=CARTESIAN_POINT('Ctrl Pts',(6.42907334018171,1.79721106794486,2.87740555063087));
#7249=CARTESIAN_POINT('Ctrl Pts',(6.43298618499128,1.82206603382117,2.94156774139178));
#7250=CARTESIAN_POINT('Ctrl Pts',(6.4368978684084,1.84691362236174,3.00571088782872));
#7251=CARTESIAN_POINT('Ctrl Pts',(6.44080955182551,1.86837774659701,3.07118752305999));
#7252=CARTESIAN_POINT('Ctrl Pts',(6.44472123524263,1.8863280242434,3.1376076648513));
#7253=CARTESIAN_POINT('Ctrl Pts',(6.44863308502627,1.90427906532715,3.20403063153584));
#7254=CARTESIAN_POINT('Ctrl Pts',(6.45254493480991,1.91871583776211,3.27139671099779));
#7255=CARTESIAN_POINT('Ctrl Pts',(6.45645678459355,1.92955835474801,3.33930267088875));
#7256=CARTESIAN_POINT('Ctrl Pts',(6.46037263616518,1.94041196353361,3.4072780979806));
#7257=CARTESIAN_POINT('Ctrl Pts',(6.46428848773681,1.94766390122192,3.47579402321336));
#7258=CARTESIAN_POINT('Ctrl Pts',(6.46820433930844,1.95128582531456,3.54443997383857));
#7259=CARTESIAN_POINT('Ctrl Pts',(6.47212245625163,1.95490984473785,3.61312563704775));
#7260=CARTESIAN_POINT('Ctrl Pts',(6.47604057319482,1.95489967004011,3.68194098549061));
#7261=CARTESIAN_POINT('Ctrl Pts',(6.47995869013801,1.95127910870616,3.75047618308761));
#7262=CARTESIAN_POINT('Ctrl Pts',(6.4838833491557,1.94765250212592,3.81912581381023));
#7263=CARTESIAN_POINT('Ctrl Pts',(6.48780800817339,1.94040352839184,3.88749387319098));
#7264=CARTESIAN_POINT('Ctrl Pts',(6.49173266719108,1.92960768452088,3.95517715759239));
#7265=CARTESIAN_POINT('Ctrl Pts',(6.49348559831366,1.92478576989576,3.98540758912064));
#7266=CARTESIAN_POINT('Ctrl Pts',(6.49523852943624,1.91925696002775,4.01550157306795));
#7267=CARTESIAN_POINT('Ctrl Pts',(6.49699146055883,1.91303120504268,4.04542412613984));
#7268=CARTESIAN_POINT('Ctrl Pts',(6.5008727175178,1.89924643361079,4.1116772240764));
#7269=CARTESIAN_POINT('Ctrl Pts',(6.50475397447678,1.88198628894892,4.17735458711251));
#7270=CARTESIAN_POINT('Ctrl Pts',(6.50863523143576,1.86131381314335,4.24205982712173));
#7271=CARTESIAN_POINT('Ctrl Pts',(6.51250998753633,1.84067596241917,4.30665668997175));
#7272=CARTESIAN_POINT('Ctrl Pts',(6.5163847436369,1.81663727951453,4.37028418844698));
#7273=CARTESIAN_POINT('Ctrl Pts',(6.52025949973747,1.78931167938922,4.43255668973963));
#7274=CARTESIAN_POINT('Ctrl Pts',(6.52413063354277,1.76201162445679,4.49477097591349));
#7275=CARTESIAN_POINT('Ctrl Pts',(6.52800176734808,1.73143094295279,4.55563231808264));
#7276=CARTESIAN_POINT('Ctrl Pts',(6.53187290115338,1.69773268329177,4.61477223114744));
#7277=CARTESIAN_POINT('Ctrl Pts',(6.53574180537595,1.66405383217141,4.67387808253015));
#7278=CARTESIAN_POINT('Ctrl Pts',(6.53961070959852,1.62726121136194,4.73126403542489));
#7279=CARTESIAN_POINT('Ctrl Pts',(6.5434796138211,1.58756426082805,4.78658528537357));
#7280=CARTESIAN_POINT('Ctrl Pts',(6.54734767812641,1.54787592827793,4.84189452539132));
#7281=CARTESIAN_POINT('Ctrl Pts',(6.55121574243173,1.50528481066992,4.89513954481636));
#7282=CARTESIAN_POINT('Ctrl Pts',(6.55508380673704,1.46004311123211,4.94600530812145));
#7283=CARTESIAN_POINT('Ctrl Pts',(6.55895498853783,1.41476494890696,4.99691206707039));
#7284=CARTESIAN_POINT('Ctrl Pts',(6.56282617033861,1.36683226981965,5.04543536161557));
#7285=CARTESIAN_POINT('Ctrl Pts',(6.56669735213939,1.31653618878333,5.09129490239415));
#7286=CARTESIAN_POINT('Ctrl Pts',(6.57057001435284,1.26622087358051,5.13717198072287));
#7287=CARTESIAN_POINT('Ctrl Pts',(6.57444267656629,1.21354074412186,5.18038295628716));
#7288=CARTESIAN_POINT('Ctrl Pts',(6.57831533877974,1.15882003527172,5.22068786935464));
#7289=CARTESIAN_POINT('Ctrl Pts',(6.58219473815397,1.10400413035407,5.26106289973798));
#7290=CARTESIAN_POINT('Ctrl Pts',(6.58607413752819,1.04714097458828,5.29852149120506));
#7291=CARTESIAN_POINT('Ctrl Pts',(6.58995353690242,0.988583156110744,5.33286750083412));
#7292=CARTESIAN_POINT('Ctrl Pts',(6.59328863359874,0.938241345920918,5.36239456216389));
#7293=CARTESIAN_POINT('Ctrl Pts',(6.59662373029505,0.88664765834881,5.38962186526931));
#7294=CARTESIAN_POINT('Ctrl Pts',(6.59995882699137,0.834037993952276,5.41445321791391));
#7295=CARTESIAN_POINT('',(6.6,1.90834530359594,4.06731613031539));
#7296=CARTESIAN_POINT('Origin',(6.6,0.,3.64739446828387));
#7297=CARTESIAN_POINT('Ctrl Pts',(6.6,1.90834530359594,4.06731613031539));
#7298=CARTESIAN_POINT('Ctrl Pts',(6.56299081980964,2.04784060254395,3.43337598697229));
#7299=CARTESIAN_POINT('Ctrl Pts',(6.48897245942892,1.64305422583221,2.02647090284419));
#7300=CARTESIAN_POINT('Ctrl Pts',(6.37794491885784,-0.472540916100214,1.38598473075093));
#7301=CARTESIAN_POINT('Ctrl Pts',(6.29024427840894,-1.80025717638368,2.51599492455183));
#7302=CARTESIAN_POINT('Ctrl Pts',(6.2395528181504,-1.9529603584434,3.4057264198301));
#7303=CARTESIAN_POINT('Ctrl Pts',(6.22587053808222,-1.95156756343269,3.64631438782879));
#7304=CARTESIAN_POINT('Origin',(1.2059437743963,0.,3.64739446828387));
#7305=CARTESIAN_POINT('',(6.599956144719,-0.42654248155568,2.15151955324975));
#7306=CARTESIAN_POINT('Ctrl Pts',(6.4559437743963,-1.5554997682929,3.6465454448856));
#7307=CARTESIAN_POINT('Ctrl Pts',(6.46061116422838,-1.55546406369716,3.58113088679472));
#7308=CARTESIAN_POINT('Ctrl Pts',(6.46527855406046,-1.55129786300922,3.51586849460407));
#7309=CARTESIAN_POINT('Ctrl Pts',(6.46994594389254,-1.54308295192937,3.45124336972736));
#7310=CARTESIAN_POINT('Ctrl Pts',(6.47464971063311,-1.53480401511366,3.38611456670539));
#7311=CARTESIAN_POINT('Ctrl Pts',(6.47935347737368,-1.52241313274287,3.32163325345467));
#7312=CARTESIAN_POINT('Ctrl Pts',(6.48405724411425,-1.50604397351761,3.25827777649169));
#7313=CARTESIAN_POINT('Ctrl Pts',(6.48836864959578,-1.4910402357253,3.20020705025716));
#7314=CARTESIAN_POINT('Ctrl Pts',(6.49268005507731,-1.47269489336211,3.14308208717692));
#7315=CARTESIAN_POINT('Ctrl Pts',(6.49699146055883,-1.45114591966537,3.0872554053374));
#7316=CARTESIAN_POINT('Ctrl Pts',(6.50128165573217,-1.42970295788867,3.03170336737719));
#7317=CARTESIAN_POINT('Ctrl Pts',(6.50557185090551,-1.40501473944522,2.97725350914402));
#7318=CARTESIAN_POINT('Ctrl Pts',(6.50986204607885,-1.37722024457809,2.92431449488931));
#7319=CARTESIAN_POINT('Ctrl Pts',(6.51396372832576,-1.35064705115635,2.87370164252155));
#7320=CARTESIAN_POINT('Ctrl Pts',(6.51806541057266,-1.32123511808883,2.8244701800106));
#7321=CARTESIAN_POINT('Ctrl Pts',(6.52216709281957,-1.28915582586842,2.77695922851613));
#7322=CARTESIAN_POINT('Ctrl Pts',(6.52626492593395,-1.25710663774667,2.72949286261793));
#7323=CARTESIAN_POINT('Ctrl Pts',(6.53036275904833,-1.22239534318046,2.68374424903125));
#7324=CARTESIAN_POINT('Ctrl Pts',(6.53446059216271,-1.18523844654547,2.64002657380317));
#7325=CARTESIAN_POINT('Ctrl Pts',(6.53855622804132,-1.14810147323584,2.59633233975415));
#7326=CARTESIAN_POINT('Ctrl Pts',(6.54265186391993,-1.10852184009623,2.55466729042924));
#7327=CARTESIAN_POINT('Ctrl Pts',(6.54674749979854,-1.06675701342171,2.51531243754776));
#7328=CARTESIAN_POINT('Ctrl Pts',(6.55084258685509,-1.02499778330378,2.47596285828235));
#7329=CARTESIAN_POINT('Ctrl Pts',(6.55493767391165,-0.981054328890206,2.4389232239911));
#7330=CARTESIAN_POINT('Ctrl Pts',(6.5590327609682,-0.935220039280021,2.40443681489053));
#7331=CARTESIAN_POINT('Ctrl Pts',(6.56313151800817,-0.889344673355695,2.36991949935319));
#7332=CARTESIAN_POINT('Ctrl Pts',(6.56723027504813,-0.841575516606041,2.33796029461034));
#7333=CARTESIAN_POINT('Ctrl Pts',(6.57132903208809,-0.792236695122554,2.30876036259954));
#7334=CARTESIAN_POINT('Ctrl Pts',(6.57542996437529,-0.74287168908268,2.27954493392215));
#7335=CARTESIAN_POINT('Ctrl Pts',(6.57953089666248,-0.691935833065455,2.25309193575008));
#7336=CARTESIAN_POINT('Ctrl Pts',(6.58363182894968,-0.639776841899525,2.22955602806261));
#7337=CARTESIAN_POINT('Ctrl Pts',(6.58773952212041,-0.587531860319731,2.20598131858089));
#7338=CARTESIAN_POINT('Ctrl Pts',(6.59184721529114,-0.534060217488819,2.18533348088132));
#7339=CARTESIAN_POINT('Ctrl Pts',(6.59595490846187,-0.479727038099651,2.16771807835392));
#7340=CARTESIAN_POINT('Ctrl Pts',(6.59728865388091,-0.46208535307097,2.1619984538715));
#7341=CARTESIAN_POINT('Ctrl Pts',(6.59862239929996,-0.444352929777357,2.15659812813977));
#7342=CARTESIAN_POINT('Ctrl Pts',(6.599956144719,-0.42654248155568,2.15151955324975));
#7343=CARTESIAN_POINT('',(6.6,-1.55328677638795,3.5644460487792));
#7344=CARTESIAN_POINT('Origin',(6.6,0.,3.64739446828387));
#7345=CARTESIAN_POINT('Ctrl Pts',(6.59414638614667,-1.55549999987963,3.64737511703584));
#7346=CARTESIAN_POINT('Ctrl Pts',(6.59510874546272,-1.55549982783689,3.63354590681215));
#7347=CARTESIAN_POINT('Ctrl Pts',(6.59607695453386,-1.55531523240308,3.61971776272618));
#7348=CARTESIAN_POINT('Ctrl Pts',(6.59802745792117,-1.5545773647494,3.59207096791355));
#7349=CARTESIAN_POINT('Ctrl Pts',(6.59900966026663,-1.55402412717383,3.5782536322402));
#7350=CARTESIAN_POINT('Ctrl Pts',(6.6,-1.55328677638795,3.5644460487792));
#7351=CARTESIAN_POINT('Ctrl Pts',(2.26863408412604,-0.684651324693825,5.04165517356951));
#7352=CARTESIAN_POINT('Ctrl Pts',(2.30564859368349,-1.14788625211098,4.81419027525137));
#7353=CARTESIAN_POINT('Ctrl Pts',(2.3796722834313,-1.8217797641733,3.86524735393602));
#7354=CARTESIAN_POINT('Ctrl Pts',(2.49070515336946,-1.17126252580745,2.23289142025749));
#7355=CARTESIAN_POINT('Ctrl Pts',(2.60173269394054,0.550929011373164,1.8972621249236));
#7356=CARTESIAN_POINT('Ctrl Pts',(2.71276023451162,1.76895437683424,3.15850697088285));
#7357=CARTESIAN_POINT('Ctrl Pts',(2.8237877750827,1.37119925940374,4.86751886652752));
#7358=CARTESIAN_POINT('Ctrl Pts',(2.93481531565378,-0.279566957660275,5.46119858728686));
#7359=CARTESIAN_POINT('Ctrl Pts',(3.04584285622486,-1.67479408727594,4.3979960058981));
#7360=CARTESIAN_POINT('Ctrl Pts',(3.15687039679593,-1.53990869075139,2.64885471465201));
#7361=CARTESIAN_POINT('Ctrl Pts',(3.26789793736702,0.00194110293598171,
1.81210655462338));
#7362=CARTESIAN_POINT('Ctrl Pts',(3.37892547793808,1.5420014927779,2.65212320530051));
#7363=CARTESIAN_POINT('Ctrl Pts',(3.48995301850917,1.67322430909778,4.40148852237912));
#7364=CARTESIAN_POINT('Ctrl Pts',(3.60098055908024,0.275705577370855,5.46186647902077));
#7365=CARTESIAN_POINT('Ctrl Pts',(3.71200809965133,-1.37370863799142,4.86446239222593));
#7366=CARTESIAN_POINT('Ctrl Pts',(3.8230356402224,-1.76803851820383,3.15508418544703));
#7367=CARTESIAN_POINT('Ctrl Pts',(3.93406318079349,-0.547003778353853,1.89550562214907));
#7368=CARTESIAN_POINT('Ctrl Pts',(4.04509072136456,1.17379929443624,2.23653514832174));
#7369=CARTESIAN_POINT('Ctrl Pts',(4.15611826193565,1.8221637133016,3.86659322783984));
#7370=CARTESIAN_POINT('Ctrl Pts',(4.26714580250671,0.805712675430428,5.29638067585463));
#7371=CARTESIAN_POINT('Ctrl Pts',(4.3781733430778,-0.946875698946845,5.2195760848642));
#7372=CARTESIAN_POINT('Ctrl Pts',(4.48920088364887,-1.83435347884445,3.70635156641869));
#7373=CARTESIAN_POINT('Ctrl Pts',(4.60022842421995,-1.04587869061767,2.13926112118895));
#7374=CARTESIAN_POINT('Ctrl Pts',(4.71125596479103,0.698160489741094,1.95007286504292));
#7375=CARTESIAN_POINT('Ctrl Pts',(4.82228350536211,1.80432722111991,3.31163848029748));
#7376=CARTESIAN_POINT('Ctrl Pts',(4.93331104593319,1.26197456066074,4.97996636915454));
#7377=CARTESIAN_POINT('Ctrl Pts',(5.04433858650427,-0.433377472991919,5.43079391382108));
#7378=CARTESIAN_POINT('Ctrl Pts',(5.15536612707534,-1.73277632833419,4.25222167463752));
#7379=CARTESIAN_POINT('Ctrl Pts',(5.26639366764643,-1.44902630832145,2.521053045387));
#7380=CARTESIAN_POINT('Ctrl Pts',(5.3774212082175,0.158619024761312,1.81895867888319));
#7381=CARTESIAN_POINT('Ctrl Pts',(5.48844874878859,1.6213501498084,2.7874193626174));
#7382=CARTESIAN_POINT('Ctrl Pts',(5.59947628935966,1.60272396252789,4.54157643737503));
#7383=CARTESIAN_POINT('Ctrl Pts',(5.71050382993074,0.119801397977272,5.4788004965795));
#7384=CARTESIAN_POINT('Ctrl Pts',(5.82153137050182,-1.47263207300637,4.74269930283736));
#7385=CARTESIAN_POINT('Ctrl Pts',(5.9325589110729,-1.71949372363033,3.00600192052272));
#7386=CARTESIAN_POINT('Ctrl Pts',(6.04358645164398,-0.395546584890944,1.8550680874704));
#7387=CARTESIAN_POINT('Ctrl Pts',(6.15461399221506,1.29018035693896,2.34215685811287));
#7388=CARTESIAN_POINT('Ctrl Pts',(6.26564153278613,1.79638565259649,4.02087081558556));
#7389=CARTESIAN_POINT('Ctrl Pts',(6.37666907335722,0.662790583736323,5.36010676734267));
#7390=CARTESIAN_POINT('Ctrl Pts',(6.48769661392829,-1.07933315373079,5.13104989888334));
#7391=CARTESIAN_POINT('Ctrl Pts',(6.56171497430901,-1.57859588144958,4.07982280745059));
#7392=CARTESIAN_POINT('Ctrl Pts',(6.59872415449937,-1.55108009138598,3.56456388988623));
#7393=CARTESIAN_POINT('Ctrl Pts',(2.34623717873851,-0.743896982560043,5.1623062111741));
#7394=CARTESIAN_POINT('Ctrl Pts',(2.38325168829595,-1.24721750834176,4.91515785201061));
#7395=CARTESIAN_POINT('Ctrl Pts',(2.45727537804376,-1.9794257610814,3.88409904831387));
#7396=CARTESIAN_POINT('Ctrl Pts',(2.56830824798192,-1.27261662587662,2.11048873057953));
#7397=CARTESIAN_POINT('Ctrl Pts',(2.67933578855301,0.598603134739513,1.74581607012819));
#7398=CARTESIAN_POINT('Ctrl Pts',(2.79036332912407,1.92202917857765,3.11620155152352));
#7399=CARTESIAN_POINT('Ctrl Pts',(2.90139086969516,1.48985469649849,4.97310118273044));
#7400=CARTESIAN_POINT('Ctrl Pts',(3.01241841026624,-0.30375902116303,5.61815441924826));
#7401=CARTESIAN_POINT('Ctrl Pts',(3.12344595083731,-1.81972081700291,4.46294860335526));
#7402=CARTESIAN_POINT('Ctrl Pts',(3.23447349140839,-1.67316323966835,2.56244701707551));
#7403=CARTESIAN_POINT('Ctrl Pts',(3.34550103197947,0.00210907445123311,
1.65329164271569));
#7404=CARTESIAN_POINT('Ctrl Pts',(3.45652857255054,1.6754371403481,2.5659983434854));
#7405=CARTESIAN_POINT('Ctrl Pts',(3.56755611312163,1.81801519954786,4.46674334146218));
#7406=CARTESIAN_POINT('Ctrl Pts',(3.6785836536927,0.29956349996529,5.61888010636462));
#7407=CARTESIAN_POINT('Ctrl Pts',(3.7896111942638,-1.49258122179998,4.96978021930246));
#7408=CARTESIAN_POINT('Ctrl Pts',(3.90063873483486,-1.92103406698283,3.11248257857215));
#7409=CARTESIAN_POINT('Ctrl Pts',(4.01166627540594,-0.594338235376009,1.74390757003961));
#7410=CARTESIAN_POINT('Ctrl Pts',(4.12269381597701,1.27537291139066,2.11444776522171));
#7411=CARTESIAN_POINT('Ctrl Pts',(4.2337213565481,1.97984293488607,3.88556138614897));
#7412=CARTESIAN_POINT('Ctrl Pts',(4.34474889711917,0.875434263318063,5.43907414500631));
#7413=CARTESIAN_POINT('Ctrl Pts',(4.45577643769026,-1.02881269618661,5.35562334103673));
#7414=CARTESIAN_POINT('Ctrl Pts',(4.56680397826132,-1.99308753031499,3.71145336340483));
#7415=CARTESIAN_POINT('Ctrl Pts',(4.67783151883243,-1.13638281854237,2.00875622172268));
#7416=CARTESIAN_POINT('Ctrl Pts',(4.78885905940349,0.758575150487437,1.80319673792884));
#7417=CARTESIAN_POINT('Ctrl Pts',(4.89988659997458,1.96046297864434,3.28258415195061));
#7418=CARTESIAN_POINT('Ctrl Pts',(5.01091414054565,1.37117834127157,5.0952792241416));
#7419=CARTESIAN_POINT('Ctrl Pts',(5.12194168111672,-0.470879384644958,5.58511870598642));
#7420=CARTESIAN_POINT('Ctrl Pts',(5.2329692216878,-1.88272049670789,4.30455982756789));
#7421=CARTESIAN_POINT('Ctrl Pts',(5.34399676225889,-1.57441643582957,2.42358615067044));
#7422=CARTESIAN_POINT('Ctrl Pts',(5.45502430282995,0.172344972748461,1.66073670909787));
#7423=CARTESIAN_POINT('Ctrl Pts',(5.56605184340105,1.76165215871761,2.7130022264108));
#7424=CARTESIAN_POINT('Ctrl Pts',(5.67707938397211,1.74141417185507,4.61895363230649));
#7425=CARTESIAN_POINT('Ctrl Pts',(5.78810692454321,0.130168299172756,5.63727949319146));
#7426=CARTESIAN_POINT('Ctrl Pts',(5.89913446511428,-1.60006490313954,4.83748047559882));
#7427=CARTESIAN_POINT('Ctrl Pts',(6.01016200568536,-1.86828849430995,2.95049962019548));
#7428=CARTESIAN_POINT('Ctrl Pts',(6.12118954625643,-0.429774836255362,1.69997081136455));
#7429=CARTESIAN_POINT('Ctrl Pts',(6.23221708682751,1.40182489957839,2.22920935023958));
#7430=CARTESIAN_POINT('Ctrl Pts',(6.34324462739859,1.95183419396477,4.05318923971664));
#7431=CARTESIAN_POINT('Ctrl Pts',(6.45427216796967,0.720144542963021,5.50831471383087));
#7432=CARTESIAN_POINT('Ctrl Pts',(6.56529970854074,-1.17273223212766,5.25943662488868));
#7433=CARTESIAN_POINT('Ctrl Pts',(6.63931806892146,-1.7151981899943,4.11724258670156));
#7434=CARTESIAN_POINT('Ctrl Pts',(6.67632724911182,-1.68530134694034,3.55739622375953));
#7435=CARTESIAN_POINT('Ctrl Pts',(2.42384027335096,-0.803142640426261,5.28295724877869));
#7436=CARTESIAN_POINT('Ctrl Pts',(2.46085478290841,-1.34654876457254,5.01612542876985));
#7437=CARTESIAN_POINT('Ctrl Pts',(2.53487847265621,-2.1370717579895,3.90295074269172));
#7438=CARTESIAN_POINT('Ctrl Pts',(2.64591134259438,-1.3739707259458,1.98808604090159));
#7439=CARTESIAN_POINT('Ctrl Pts',(2.75693888316546,0.646277258105862,1.59437001533278));
#7440=CARTESIAN_POINT('Ctrl Pts',(2.86796642373654,2.07510398032106,3.07389613216417));
#7441=CARTESIAN_POINT('Ctrl Pts',(2.97899396430762,1.60851013359324,5.07868349893336));
#7442=CARTESIAN_POINT('Ctrl Pts',(3.09002150487869,-0.327951084665789,5.77511025120965));
#7443=CARTESIAN_POINT('Ctrl Pts',(3.20104904544978,-1.96464754672989,4.52790120081243));
#7444=CARTESIAN_POINT('Ctrl Pts',(3.31207658602085,-1.80641778858531,2.47603931949901));
#7445=CARTESIAN_POINT('Ctrl Pts',(3.42310412659193,0.00227704596648382,
1.494476730808));
#7446=CARTESIAN_POINT('Ctrl Pts',(3.53413166716301,1.8088727879183,2.47987348167028));
#7447=CARTESIAN_POINT('Ctrl Pts',(3.64515920773409,1.96280608999794,4.53199816054524));
#7448=CARTESIAN_POINT('Ctrl Pts',(3.75618674830517,0.323421422559726,5.77589373370847));
#7449=CARTESIAN_POINT('Ctrl Pts',(3.86721428887625,-1.61145380560854,5.07509804637899));
#7450=CARTESIAN_POINT('Ctrl Pts',(3.97824182944732,-2.07402961576183,3.06988097169728));
#7451=CARTESIAN_POINT('Ctrl Pts',(4.08926937001841,-0.641672692398164,1.59230951793014));
#7452=CARTESIAN_POINT('Ctrl Pts',(4.20029691058948,1.37694652834506,1.99236038212167));
#7453=CARTESIAN_POINT('Ctrl Pts',(4.31132445116056,2.13752215647056,3.90452954445811));
#7454=CARTESIAN_POINT('Ctrl Pts',(4.42235199173164,0.9451558512057,5.58176761415798));
#7455=CARTESIAN_POINT('Ctrl Pts',(4.53337953230272,-1.11074969342638,5.49167059720925));
#7456=CARTESIAN_POINT('Ctrl Pts',(4.64440707287379,-2.15182158178555,3.71655516039097));
#7457=CARTESIAN_POINT('Ctrl Pts',(4.75543461344488,-1.22688694646707,1.8782513222564));
#7458=CARTESIAN_POINT('Ctrl Pts',(4.86646215401595,0.818989811233778,1.65632061081476));
#7459=CARTESIAN_POINT('Ctrl Pts',(4.97748969458703,2.11659873616878,3.25352982360373));
#7460=CARTESIAN_POINT('Ctrl Pts',(5.08851723515811,1.48038212188239,5.21059207912866));
#7461=CARTESIAN_POINT('Ctrl Pts',(5.19954477572919,-0.508381296297998,5.73944349815176));
#7462=CARTESIAN_POINT('Ctrl Pts',(5.31057231630027,-2.0326646650816,4.35689798049827));
#7463=CARTESIAN_POINT('Ctrl Pts',(5.42159985687135,-1.69980656333768,2.32611925595385));
#7464=CARTESIAN_POINT('Ctrl Pts',(5.53262739744242,0.186070920735613,1.50251473931255));
#7465=CARTESIAN_POINT('Ctrl Pts',(5.64365493801351,1.90195416762681,2.63858509020417));
#7466=CARTESIAN_POINT('Ctrl Pts',(5.75468247858458,1.88010438118225,4.69633082723795));
#7467=CARTESIAN_POINT('Ctrl Pts',(5.86571001915567,0.140535200368236,5.79575848980343));
#7468=CARTESIAN_POINT('Ctrl Pts',(5.97673755972673,-1.72749773327271,4.9322616483603));
#7469=CARTESIAN_POINT('Ctrl Pts',(6.08776510029783,-2.01708326498956,2.89499731986824));
#7470=CARTESIAN_POINT('Ctrl Pts',(6.19879264086889,-0.464003087619777,1.54487353525871));
#7471=CARTESIAN_POINT('Ctrl Pts',(6.30982018143998,1.51346944221782,2.1162618423663));
#7472=CARTESIAN_POINT('Ctrl Pts',(6.42084772201105,2.10728273533306,4.08550766384771));
#7473=CARTESIAN_POINT('Ctrl Pts',(6.53187526258214,0.777498502189718,5.65652266031908));
#7474=CARTESIAN_POINT('Ctrl Pts',(6.64290280315321,-1.26613131052453,5.38782335089402));
#7475=CARTESIAN_POINT('Ctrl Pts',(6.71692116353393,-1.85180049853903,4.15466236595253));
#7476=CARTESIAN_POINT('Ctrl Pts',(6.75393034372429,-1.81952260249468,3.55022855763283));
#7477=CARTESIAN_POINT('Ctrl Pts',(2.50144336796343,-0.862388298292479,5.40360828638327));
#7478=CARTESIAN_POINT('Ctrl Pts',(2.53845787752087,-1.44588002080332,5.11709300552908));
#7479=CARTESIAN_POINT('Ctrl Pts',(2.61248156726868,-2.29471775489761,3.92180243706957));
#7480=CARTESIAN_POINT('Ctrl Pts',(2.72351443720684,-1.47532482601497,1.86568335122363));
#7481=CARTESIAN_POINT('Ctrl Pts',(2.83454197777792,0.69395138147221,1.44292396053739));
#7482=CARTESIAN_POINT('Ctrl Pts',(2.945569518349,2.22817878206446,3.03159071280484));
#7483=CARTESIAN_POINT('Ctrl Pts',(3.05659705892007,1.72716557068799,5.18426581513628));
#7484=CARTESIAN_POINT('Ctrl Pts',(3.16762459949115,-0.352143148168544,5.93206608317104));
#7485=CARTESIAN_POINT('Ctrl Pts',(3.27865214006223,-2.10957427645686,4.5928537982696));
#7486=CARTESIAN_POINT('Ctrl Pts',(3.38967968063331,-1.93967233750227,2.38963162192252));
#7487=CARTESIAN_POINT('Ctrl Pts',(3.50070722120439,0.00244501748173489,
1.33566181890031));
#7488=CARTESIAN_POINT('Ctrl Pts',(3.61173476177546,1.94230843548851,2.39374861985516));
#7489=CARTESIAN_POINT('Ctrl Pts',(3.72276230234655,2.10759698044802,4.59725297962832));
#7490=CARTESIAN_POINT('Ctrl Pts',(3.83378984291762,0.34727934515416,5.93290736105231));
#7491=CARTESIAN_POINT('Ctrl Pts',(3.9448173834887,-1.73032638941711,5.18041587345552));
#7492=CARTESIAN_POINT('Ctrl Pts',(4.05584492405978,-2.22702516454082,3.0272793648224));
#7493=CARTESIAN_POINT('Ctrl Pts',(4.16687246463086,-0.689007149420319,1.44071146582068));
#7494=CARTESIAN_POINT('Ctrl Pts',(4.27790000520194,1.47852014529947,1.87027299902164));
#7495=CARTESIAN_POINT('Ctrl Pts',(4.38892754577301,2.29520137805504,3.92349770276724));
#7496=CARTESIAN_POINT('Ctrl Pts',(4.4999550863441,1.01487743909333,5.72446108330965));
#7497=CARTESIAN_POINT('Ctrl Pts',(4.61098262691517,-1.19268669066615,5.62771785338177));
#7498=CARTESIAN_POINT('Ctrl Pts',(4.72201016748625,-2.31055563325609,3.72165695737712));
#7499=CARTESIAN_POINT('Ctrl Pts',(4.83303770805733,-1.31739107439176,1.74774642279012));
#7500=CARTESIAN_POINT('Ctrl Pts',(4.94406524862841,0.879404471980121,1.50944448370068));
#7501=CARTESIAN_POINT('Ctrl Pts',(5.05509278919948,2.2727344936932,3.22447549525686));
#7502=CARTESIAN_POINT('Ctrl Pts',(5.16612032977057,1.58958590249323,5.32590493411573));
#7503=CARTESIAN_POINT('Ctrl Pts',(5.27714787034164,-0.545883207951038,5.89376829031711));
#7504=CARTESIAN_POINT('Ctrl Pts',(5.38817541091273,-2.1826088334553,4.40923613342865));
#7505=CARTESIAN_POINT('Ctrl Pts',(5.4992029514838,-1.82519669084581,2.22865236123728));
#7506=CARTESIAN_POINT('Ctrl Pts',(5.61023049205488,0.199796868722764,1.34429276952724));
#7507=CARTESIAN_POINT('Ctrl Pts',(5.72125803262597,2.042256176536,2.56416795399757));
#7508=CARTESIAN_POINT('Ctrl Pts',(5.83228557319703,2.01879459050943,4.77370802216941));
#7509=CARTESIAN_POINT('Ctrl Pts',(5.94331311376813,0.150902101563718,5.95423748641541));
#7510=CARTESIAN_POINT('Ctrl Pts',(6.05434065433919,-1.85493056340588,5.02704282112175));
#7511=CARTESIAN_POINT('Ctrl Pts',(6.16536819491027,-2.16587803566918,2.83949501954101));
#7512=CARTESIAN_POINT('Ctrl Pts',(6.27639573548135,-0.498231338984194,1.38977625915286));
#7513=CARTESIAN_POINT('Ctrl Pts',(6.38742327605243,1.62511398485724,2.00331433449301));
#7514=CARTESIAN_POINT('Ctrl Pts',(6.49845081662351,2.26273127670134,4.1178260879788));
#7515=CARTESIAN_POINT('Ctrl Pts',(6.60947835719459,0.834852461416416,5.80473060680729));
#7516=CARTESIAN_POINT('Ctrl Pts',(6.72050589776567,-1.3595303889214,5.51621007689934));
#7517=CARTESIAN_POINT('Ctrl Pts',(6.79452425814639,-1.98840280708376,4.1920821452035));
#7518=CARTESIAN_POINT('Ctrl Pts',(6.83153343833676,-1.95374385804904,3.54306089150614));
#7519=CARTESIAN_POINT('Ctrl Pts',(6.6,0.83475068776765,5.41764852956582));
#7520=CARTESIAN_POINT('Ctrl Pts',(6.6,0.7907192463387,5.43356975418934));
#7521=CARTESIAN_POINT('Ctrl Pts',(6.6,0.746172855022355,5.44776191297247));
#7522=CARTESIAN_POINT('Ctrl Pts',(6.6,0.701168580024064,5.46015373566206));
#7523=CARTESIAN_POINT('Ctrl Pts',(6.59999999999999,0.632780325132891,5.47898428295328));
#7524=CARTESIAN_POINT('Ctrl Pts',(6.6,0.563334570934092,5.4936600771938));
#7525=CARTESIAN_POINT('Ctrl Pts',(6.6,0.493183000021699,5.50428783505599));
#7526=CARTESIAN_POINT('Ctrl Pts',(6.6,0.422101207198843,5.51505651881754));
#7527=CARTESIAN_POINT('Ctrl Pts',(6.6,0.350293636793038,5.52166884246508));
#7528=CARTESIAN_POINT('Ctrl Pts',(6.6,0.27813252516632,5.52418340588879));
#7529=CARTESIAN_POINT('Ctrl Pts',(6.6,0.245886653870964,5.5253070622003));
#7530=CARTESIAN_POINT('Ctrl Pts',(6.6,0.213570373230081,5.52561179547265));
#7531=CARTESIAN_POINT('Ctrl Pts',(6.6,0.181218209310509,5.52509972733514));
#7532=CARTESIAN_POINT('Ctrl Pts',(6.6,0.160635756760572,5.52477394949324));
#7533=CARTESIAN_POINT('Ctrl Pts',(6.6,0.140038799819156,5.52411753323207));
#7534=CARTESIAN_POINT('Ctrl Pts',(6.6,0.119436477971668,5.52313064631116));
#7535=CARTESIAN_POINT('Ctrl Pts',(6.6,0.107012385202456,5.5225355107362));
#7536=CARTESIAN_POINT('Ctrl Pts',(6.6,0.0945852684045237,5.52182002860968));
#7537=CARTESIAN_POINT('Ctrl Pts',(6.6,0.0821742362622182,5.52098560168444));
#7538=CARTESIAN_POINT('Ctrl Pts',(6.6,0.0118828483352063,5.51625972344755));
#7539=CARTESIAN_POINT('Ctrl Pts',(6.6,-0.0580208766357301,5.50771766688684));
#7540=CARTESIAN_POINT('Ctrl Pts',(6.6,-0.127194914653041,5.49545172311728));
#7541=CARTESIAN_POINT('Ctrl Pts',(6.6,-0.195407928455584,5.48335618820801));
#7542=CARTESIAN_POINT('Ctrl Pts',(6.6,-0.262912350188068,5.46763903161646));
#7543=CARTESIAN_POINT('Ctrl Pts',(6.6,-0.329361205530838,5.44834294016328));
#7544=CARTESIAN_POINT('Ctrl Pts',(6.6,-0.39443868562668,5.42944508254039));
#7545=CARTESIAN_POINT('Ctrl Pts',(6.6,-0.458504499770776,5.40711402878201));
#7546=CARTESIAN_POINT('Ctrl Pts',(6.6,-0.521201674010066,5.38135263368021));
#7547=CARTESIAN_POINT('Ctrl Pts',(6.6,-0.536341223469168,5.37513200380317));
#7548=CARTESIAN_POINT('Ctrl Pts',(6.6,-0.551400795462264,5.36871120070083));
#7549=CARTESIAN_POINT('Ctrl Pts',(6.6,-0.566375007959067,5.36208997493157));
#7550=CARTESIAN_POINT('Ctrl Pts',(6.6,-0.580397210895579,5.35588970420315));
#7551=CARTESIAN_POINT('Ctrl Pts',(6.6,-0.594348562079377,5.34951165292965));
#7552=CARTESIAN_POINT('Ctrl Pts',(6.6,-0.608198751037917,5.34296812914935));
#7553=CARTESIAN_POINT('Ctrl Pts',(6.6,-0.668835467720879,5.31432030356649));
#7554=CARTESIAN_POINT('Ctrl Pts',(6.6,-0.727626283845795,5.2824663680222));
#7555=CARTESIAN_POINT('Ctrl Pts',(6.6,-0.784252300272617,5.24745318929936));
#7556=CARTESIAN_POINT('Ctrl Pts',(6.6,-0.839181587060244,5.21348913784788));
#7557=CARTESIAN_POINT('Ctrl Pts',(6.6,-0.892074481393698,5.17655181647775));
#7558=CARTESIAN_POINT('Ctrl Pts',(6.6,-0.942605638289231,5.13664980579598));
#7559=CARTESIAN_POINT('Ctrl Pts',(6.6,-0.97196789287341,5.11346385344422));
#7560=CARTESIAN_POINT('Ctrl Pts',(6.6,-1.0005320279455,5.08927628731349));
#7561=CARTESIAN_POINT('Ctrl Pts',(6.6,-1.02822743693251,5.06408422531173));
#7562=CARTESIAN_POINT('Ctrl Pts',(6.6,-1.05360839269705,5.0409974165347));
#7563=CARTESIAN_POINT('Ctrl Pts',(6.6,-1.0782596465578,5.01706684049449));
#7564=CARTESIAN_POINT('Ctrl Pts',(6.6,-1.10215906011825,4.99233467734655));
#7565=CARTESIAN_POINT('Ctrl Pts',(6.6,-1.11213104593841,4.98201522831115));
#7566=CARTESIAN_POINT('Ctrl Pts',(6.6,-1.12197209812286,4.97155621624695));
#7567=CARTESIAN_POINT('Ctrl Pts',(6.6,-1.13168042863728,4.96096067320925));
#7568=CARTESIAN_POINT('Ctrl Pts',(6.6,-1.13846377682764,4.95355741704859));
#7569=CARTESIAN_POINT('Ctrl Pts',(6.6,-1.14518055031752,4.94608936896101));
#7570=CARTESIAN_POINT('Ctrl Pts',(6.6,-1.15182470155627,4.93856413467273));
#7571=CARTESIAN_POINT('Ctrl Pts',(6.6,-1.19473914758542,4.88995879004454));
#7572=CARTESIAN_POINT('Ctrl Pts',(6.6,-1.23469798302823,4.83889366788672));
#7573=CARTESIAN_POINT('Ctrl Pts',(6.6,-1.27161691617958,4.78569376443529));
#7574=CARTESIAN_POINT('Ctrl Pts',(6.6,-1.30884832150702,4.73204359094136));
#7575=CARTESIAN_POINT('Ctrl Pts',(6.6,-1.34298845602856,4.67622123916325));
#7576=CARTESIAN_POINT('Ctrl Pts',(6.6,-1.37390225462564,4.61854045629316));
#7577=CARTESIAN_POINT('Ctrl Pts',(6.6,-1.39543358791776,4.57836602879194));
#7578=CARTESIAN_POINT('Ctrl Pts',(6.6,-1.41539879072854,4.53728964557128));
#7579=CARTESIAN_POINT('Ctrl Pts',(6.6,-1.43373730300016,4.49541608744732));
#7580=CARTESIAN_POINT('Ctrl Pts',(6.6,-1.44483372953756,4.47007887062731));
#7581=CARTESIAN_POINT('Ctrl Pts',(6.6,-1.45533433096051,4.44444978199303));
#7582=CARTESIAN_POINT('Ctrl Pts',(6.6,-1.46522340819265,4.4185523449034));
#7583=CARTESIAN_POINT('Ctrl Pts',(6.6,-1.47150797518841,4.40209437065686));
#7584=CARTESIAN_POINT('Ctrl Pts',(6.6,-1.47754607716869,4.38552568952892));
#7585=CARTESIAN_POINT('Ctrl Pts',(6.6,-1.48332362301664,4.36888265218315));
#7586=CARTESIAN_POINT('Ctrl Pts',(6.6,-1.50409466260666,4.30904873710829));
#7587=CARTESIAN_POINT('Ctrl Pts',(6.6,-1.52153669760017,4.24816653118245));
#7588=CARTESIAN_POINT('Ctrl Pts',(6.6,-1.53551151713138,4.1865281437664));
#7589=CARTESIAN_POINT('Ctrl Pts',(6.6,-1.54677461255909,4.13685029011493));
#7590=CARTESIAN_POINT('Ctrl Pts',(6.6,-1.55578462243918,4.0866809055628));
#7591=CARTESIAN_POINT('Ctrl Pts',(6.6,-1.5624447079276,4.03617640078013));
#7592=CARTESIAN_POINT('Ctrl Pts',(6.6,-1.56482594198486,4.01811911802562));
#7593=CARTESIAN_POINT('Ctrl Pts',(6.6,-1.56690656930183,4.0000190527265));
#7594=CARTESIAN_POINT('Ctrl Pts',(6.6,-1.56868146275449,3.98188358890452));
#7595=CARTESIAN_POINT('Ctrl Pts',(6.6,-1.56996504110089,3.96876827281105));
#7596=CARTESIAN_POINT('Ctrl Pts',(6.6,-1.57108783614685,3.95564316697099));
#7597=CARTESIAN_POINT('Ctrl Pts',(6.6,-1.57204829871556,3.94251393056363));
#7598=CARTESIAN_POINT('Ctrl Pts',(6.6,-1.57651492193096,3.88145652546695));
#7599=CARTESIAN_POINT('Ctrl Pts',(6.6,-1.57747688601606,3.8202878692938));
#7600=CARTESIAN_POINT('Ctrl Pts',(6.6,-1.57477701172204,3.75928439565726));
#7601=CARTESIAN_POINT('Ctrl Pts',(6.6,-1.57207713742801,3.69828092202073));
#7602=CARTESIAN_POINT('Ctrl Pts',(6.6,-1.56571553600282,3.63744172304545));
#7603=CARTESIAN_POINT('Ctrl Pts',(6.6,-1.55548296577373,3.57706412386904));
#7604=CARTESIAN_POINT('Ctrl Pts',(6.6,-1.55476975631725,3.57285580926891));
#7605=CARTESIAN_POINT('Ctrl Pts',(6.6,-1.55403772001803,3.56864974883175));
#7606=CARTESIAN_POINT('Ctrl Pts',(6.6,-1.55328677638795,3.5644460487792));
#7607=CARTESIAN_POINT('Ctrl Pts',(2.5,-0.90555138132905,2.37953274318763));
#7608=CARTESIAN_POINT('Ctrl Pts',(2.5,-0.93880750735117,2.39730741392822));
#7609=CARTESIAN_POINT('Ctrl Pts',(2.5,-0.971294169096419,2.41632950410138));
#7610=CARTESIAN_POINT('Ctrl Pts',(2.5,-1.00293325234873,2.43657864884141));
#7611=CARTESIAN_POINT('Ctrl Pts',(2.5,-1.05381727266378,2.46914463326318));
#7612=CARTESIAN_POINT('Ctrl Pts',(2.5,-1.10251035681737,2.504881140639));
#7613=CARTESIAN_POINT('Ctrl Pts',(2.5,-1.14893834404752,2.54343425063693));
#7614=CARTESIAN_POINT('Ctrl Pts',(2.5,-1.19536633127767,2.58198736063487));
#7615=CARTESIAN_POINT('Ctrl Pts',(2.5,-1.23952977771182,2.62335775774592));
#7616=CARTESIAN_POINT('Ctrl Pts',(2.5,-1.28133554406986,2.66724270313463));
#7617=CARTESIAN_POINT('Ctrl Pts',(2.5,-1.30007944324187,2.68691881634089));
#7618=CARTESIAN_POINT('Ctrl Pts',(2.5,-1.31834908791515,2.70710103623637));
#7619=CARTESIAN_POINT('Ctrl Pts',(2.5,-1.33613438528023,2.72776484851289));
#7620=CARTESIAN_POINT('Ctrl Pts',(2.5,-1.34511395963603,2.73819774907128));
#7621=CARTESIAN_POINT('Ctrl Pts',(2.5,-1.3539700498305,2.7487534378352));
#7622=CARTESIAN_POINT('Ctrl Pts',(2.5,-1.36270123656446,2.75942890284035));
#7623=CARTESIAN_POINT('Ctrl Pts',(2.5,-1.37087012055391,2.76941685039178));
#7624=CARTESIAN_POINT('Ctrl Pts',(2.5,-1.37893068792576,2.77951115670231));
#7625=CARTESIAN_POINT('Ctrl Pts',(2.5,-1.3868685316678,2.78969190448424));
#7626=CARTESIAN_POINT('Ctrl Pts',(2.5,-1.42575294050728,2.83956342777312));
#7627=CARTESIAN_POINT('Ctrl Pts',(2.5,-1.46176828378797,2.89159377977689));
#7628=CARTESIAN_POINT('Ctrl Pts',(2.5,-1.49483280838799,2.94542719134683));
#7629=CARTESIAN_POINT('Ctrl Pts',(2.5,-1.52879779255553,3.00072666998067));
#7630=CARTESIAN_POINT('Ctrl Pts',(2.5,-1.55964980038297,3.0579294097504));
#7631=CARTESIAN_POINT('Ctrl Pts',(2.5,-1.5872713657029,3.1166972983774));
#7632=CARTESIAN_POINT('Ctrl Pts',(2.5,-1.61427745983938,3.17415570502743));
#7633=CARTESIAN_POINT('Ctrl Pts',(2.5,-1.63819595312948,3.23311127180302));
#7634=CARTESIAN_POINT('Ctrl Pts',(2.5,-1.65888103082398,3.29327996689751));
#7635=CARTESIAN_POINT('Ctrl Pts',(2.5,-1.66330526486958,3.30614916629079));
#7636=CARTESIAN_POINT('Ctrl Pts',(2.5,-1.66758143129416,3.31907395081593));
#7637=CARTESIAN_POINT('Ctrl Pts',(2.5,-1.67170785006544,3.33205167100484));
#7638=CARTESIAN_POINT('Ctrl Pts',(2.5,-1.67470502409831,3.34147788005242));
#7639=CARTESIAN_POINT('Ctrl Pts',(2.5,-1.67762270873155,3.35093067258331));
#7640=CARTESIAN_POINT('Ctrl Pts',(2.5,-1.68045765020628,3.36039960232082));
#7641=CARTESIAN_POINT('Ctrl Pts',(2.5,-1.69969107444953,3.42464076722468));
#7642=CARTESIAN_POINT('Ctrl Pts',(2.5,-1.71515655757218,3.48973852410454));
#7643=CARTESIAN_POINT('Ctrl Pts',(2.5,-1.72674329036456,3.55533433283122));
#7644=CARTESIAN_POINT('Ctrl Pts',(2.5,-1.73830533428164,3.62079037077252));
#7645=CARTESIAN_POINT('Ctrl Pts',(2.5,-1.74600577016652,3.68674333672573));
#7646=CARTESIAN_POINT('Ctrl Pts',(2.5,-1.74969313315652,3.75286685210673));
#7647=CARTESIAN_POINT('Ctrl Pts',(2.5,-1.75158782641292,3.78684337652853));
#7648=CARTESIAN_POINT('Ctrl Pts',(2.5,-1.75242223721534,3.82086532262759));
#7649=CARTESIAN_POINT('Ctrl Pts',(2.5,-1.75217071705448,3.85489016933049));
#7650=CARTESIAN_POINT('Ctrl Pts',(2.5,-1.75188640575889,3.89335089635671));
#7651=CARTESIAN_POINT('Ctrl Pts',(2.5,-1.75021469129045,3.93181536987594));
#7652=CARTESIAN_POINT('Ctrl Pts',(2.5,-1.74719268051567,3.97023541010561));
#7653=CARTESIAN_POINT('Ctrl Pts',(2.5,-1.74626233628244,3.98206325108041));
#7654=CARTESIAN_POINT('Ctrl Pts',(2.5,-1.74520379368855,3.99388863700969));
#7655=CARTESIAN_POINT('Ctrl Pts',(2.5,-1.74401857389237,4.00570464324205));
#7656=CARTESIAN_POINT('Ctrl Pts',(2.5,-1.73746351572078,4.07105506048821));
#7657=CARTESIAN_POINT('Ctrl Pts',(2.5,-1.72706359835322,4.13587276899823));
#7658=CARTESIAN_POINT('Ctrl Pts',(2.5,-1.71308067358899,4.19991291679085));
#7659=CARTESIAN_POINT('Ctrl Pts',(2.5,-1.69878949243908,4.26536484250758));
#7660=CARTESIAN_POINT('Ctrl Pts',(2.5,-1.68075547676008,4.33000530229676));
#7661=CARTESIAN_POINT('Ctrl Pts',(2.5,-1.65920408579077,4.39358324301916));
#7662=CARTESIAN_POINT('Ctrl Pts',(2.5,-1.63719262963768,4.45851840458285));
#7663=CARTESIAN_POINT('Ctrl Pts',(2.5,-1.6115118634901,4.52234611045107));
#7664=CARTESIAN_POINT('Ctrl Pts',(2.5,-1.58234824099336,4.58479677198594));
#7665=CARTESIAN_POINT('Ctrl Pts',(2.5,-1.57482933895901,4.6008976663832));
#7666=CARTESIAN_POINT('Ctrl Pts',(2.5,-1.56707866594256,4.61690697691865));
#7667=CARTESIAN_POINT('Ctrl Pts',(2.5,-1.55909887661223,4.63281994276844));
#7668=CARTESIAN_POINT('Ctrl Pts',(2.5,-1.55322527454176,4.64453283709354));
#7669=CARTESIAN_POINT('Ctrl Pts',(2.5,-1.54722753641133,4.65619353199876));
#7670=CARTESIAN_POINT('Ctrl Pts',(2.5,-1.5411066480093,4.66780009870029));
#7671=CARTESIAN_POINT('Ctrl Pts',(2.5,-1.53534542546513,4.67872465888653));
#7672=CARTESIAN_POINT('Ctrl Pts',(2.5,-1.52947966958375,4.68959258357274));
#7673=CARTESIAN_POINT('Ctrl Pts',(2.5,-1.52351124623624,4.70040147771323));
#7674=CARTESIAN_POINT('Ctrl Pts',(2.5,-1.48912287726794,4.76267927173023));
#7675=CARTESIAN_POINT('Ctrl Pts',(2.5,-1.4513252131105,4.82300799807137));
#7676=CARTESIAN_POINT('Ctrl Pts',(2.5,-1.41034991340656,4.88110430172282));
#7677=CARTESIAN_POINT('Ctrl Pts',(2.5,-1.37394992444786,4.93271355965951));
#7678=CARTESIAN_POINT('Ctrl Pts',(2.5,-1.33504133706495,4.982561572211));
#7679=CARTESIAN_POINT('Ctrl Pts',(2.5,-1.29375331926984,5.03044054309444));
#7680=CARTESIAN_POINT('Ctrl Pts',(2.5,-1.28165188881147,5.04447376792591));
#7681=CARTESIAN_POINT('Ctrl Pts',(2.5,-1.26934585898454,5.05833775135132));
#7682=CARTESIAN_POINT('Ctrl Pts',(2.5,-1.25683802017703,5.07202700942535));
#7683=CARTESIAN_POINT('Ctrl Pts',(2.5,-1.2467077044287,5.0831141771435));
#7684=CARTESIAN_POINT('Ctrl Pts',(2.5,-1.23645016461734,5.09408100911092));
#7685=CARTESIAN_POINT('Ctrl Pts',(2.5,-1.22607160176172,5.10492048819118));
#7686=CARTESIAN_POINT('Ctrl Pts',(2.5,-1.17589217237818,5.15732840657345));
#7687=CARTESIAN_POINT('Ctrl Pts',(2.5,-1.12285728917657,5.20679395228197));
#7688=CARTESIAN_POINT('Ctrl Pts',(2.5,-1.0671763087449,5.25302071945437));
#7689=CARTESIAN_POINT('Ctrl Pts',(2.5,-1.01196398502003,5.29885840431713));
#7690=CARTESIAN_POINT('Ctrl Pts',(2.5,-0.954149411695466,5.3415125564613));
#7691=CARTESIAN_POINT('Ctrl Pts',(2.5,-0.893894163872906,5.38066677881512));
#7692=CARTESIAN_POINT('Ctrl Pts',(2.5,-0.883181709014017,5.38762779639712));
#7693=CARTESIAN_POINT('Ctrl Pts',(2.5,-0.872392012796053,5.39447809860179));
#7694=CARTESIAN_POINT('Ctrl Pts',(2.5,-0.861525859670531,5.40121577991141));
#7695=CARTESIAN_POINT('Ctrl Pts',(2.2684956023837,1.13599383904839,2.05457297837212));
#7696=CARTESIAN_POINT('Ctrl Pts',(2.30551665559472,1.66530114882627,2.43205274651924));
#7697=CARTESIAN_POINT('Ctrl Pts',(2.37954688899609,2.30874613777931,3.74944295559739));
#7698=CARTESIAN_POINT('Ctrl Pts',(2.49058630258783,1.16608200062918,5.64507475471972));
#7699=CARTESIAN_POINT('Ctrl Pts',(2.60161384315891,-1.04293058450782,5.7096573157296));
#7700=CARTESIAN_POINT('Ctrl Pts',(2.71264138372999,-2.2985040575111,3.89288000979708));
#7701=CARTESIAN_POINT('Ctrl Pts',(2.82366892430106,-1.45435102275404,1.85036189287024));
#7702=CARTESIAN_POINT('Ctrl Pts',(2.93469646487215,0.718720235097674,1.4504525726535));
#7703=CARTESIAN_POINT('Ctrl Pts',(3.04572400544322,2.23505443062616,3.05738160024003));
#7704=CARTESIAN_POINT('Ctrl Pts',(3.15675154601431,1.70937833319429,5.20357835530822));
#7705=CARTESIAN_POINT('Ctrl Pts',(3.26777908658538,-0.378088709672632,5.92786550335696));
#7706=CARTESIAN_POINT('Ctrl Pts',(3.37880662715646,-2.12010467341404,4.56866108547329));
#7707=CARTESIAN_POINT('Ctrl Pts',(3.48983416772754,-1.92509810864168,2.36771502264023));
#7708=CARTESIAN_POINT('Ctrl Pts',(3.60086170829862,0.0287726246970394,1.3359598329503));
#7709=CARTESIAN_POINT('Ctrl Pts',(3.7118892488697,1.95635373610663,2.41603341962473));
#7710=CARTESIAN_POINT('Ctrl Pts',(3.82291678944078,2.0965179233959,4.62114101481739));
#7711=CARTESIAN_POINT('Ctrl Pts',(3.93394433001185,0.321203270128675,5.93658538901197));
#7712=CARTESIAN_POINT('Ctrl Pts',(4.04497187058293,-1.74757773142461,5.16051723839122));
#7713=CARTESIAN_POINT('Ctrl Pts',(4.15599941115401,-2.2196887832987,3.00198764182795));
#7714=CARTESIAN_POINT('Ctrl Pts',(4.26702695172509,-0.663786606567354,1.43313269957975));
#7715=CARTESIAN_POINT('Ctrl Pts',(4.37805449229617,1.49858251767498,1.88733236901576));
#7716=CARTESIAN_POINT('Ctrl Pts',(4.48908203286725,2.29177547185453,3.949608535076));
#7717=CARTESIAN_POINT('Ctrl Pts',(4.60010957343832,0.991093389100879,5.73576745544));
#7718=CARTESIAN_POINT('Ctrl Pts',(4.7111371140094,-1.21509863142361,5.61388972183788));
#7719=CARTESIAN_POINT('Ctrl Pts',(4.82216465458049,-2.3111189503039,3.69532819685544));
#7720=CARTESIAN_POINT('Ctrl Pts',(4.93319219515156,-1.29559086556015,1.73297264398223));
#7721=CARTESIAN_POINT('Ctrl Pts',(5.04421973572264,0.903650040337952,1.51972289010189));
#7722=CARTESIAN_POINT('Ctrl Pts',(5.15524727629372,2.27727441159882,3.25041685278073));
#7723=CARTESIAN_POINT('Ctrl Pts',(5.26627481686479,1.57027056200704,5.34380488426394));
#7724=CARTESIAN_POINT('Ctrl Pts',(5.37730235743588,-0.571403078011826,5.88727855768163));
#7725=CARTESIAN_POINT('Ctrl Pts',(5.48832989800695,-2.19102344350068,4.38427456450717));
#7726=CARTESIAN_POINT('Ctrl Pts',(5.59935743857804,-1.80880579267535,2.20804710973091));
#7727=CARTESIAN_POINT('Ctrl Pts',(5.71038497914911,0.225994198385467,1.34682732113855));
#7728=CARTESIAN_POINT('Ctrl Pts',(5.82141251972019,2.05437013573577,2.5876082456352));
#7729=CARTESIAN_POINT('Ctrl Pts',(5.93244006029126,2.00567014672563,4.79648094529437));
#7730=CARTESIAN_POINT('Ctrl Pts',(6.04346760086235,0.124697940094911,5.95583840267335));
#7731=CARTESIAN_POINT('Ctrl Pts',(6.15449514143342,-1.87059546628156,5.00542858236713));
#7732=CARTESIAN_POINT('Ctrl Pts',(6.2655226820045,-2.15606965103839,2.81553154933147));
#7733=CARTESIAN_POINT('Ctrl Pts',(6.37655022257558,-0.473125107460962,1.3831890024094));
#7734=CARTESIAN_POINT('Ctrl Pts',(6.48757776314666,1.64508549561477,2.02446699268324));
#7735=CARTESIAN_POINT('Ctrl Pts',(6.56159612352738,2.0503723003236,3.43311140089402));
#7736=CARTESIAN_POINT('Ctrl Pts',(6.59860530371774,1.91070454657702,4.06783526971427));
#7737=CARTESIAN_POINT('Ctrl Pts',(2.34618472182287,1.05786062916686,2.16412661457789));
#7738=CARTESIAN_POINT('Ctrl Pts',(2.38320577503389,1.55076239015994,2.51564347259569));
#7739=CARTESIAN_POINT('Ctrl Pts',(2.45723600843527,2.14995148560286,3.74242410073808));
#7740=CARTESIAN_POINT('Ctrl Pts',(2.56827542202699,1.08587933881672,5.50767508957099));
#7741=CARTESIAN_POINT('Ctrl Pts',(2.67930296259808,-0.971198228706072,5.56781568741114));
#7742=CARTESIAN_POINT('Ctrl Pts',(2.79033050316915,-2.14041385159106,3.87599561071092));
#7743=CARTESIAN_POINT('Ctrl Pts',(2.90135804374023,-1.35432133086994,1.97396108729576));
#7744=CARTESIAN_POINT('Ctrl Pts',(3.01238558431131,0.669286939735766,1.60155737298641));
#7745=CARTESIAN_POINT('Ctrl Pts',(3.12341312488239,2.08132826511188,3.09796245346921));
#7746=CARTESIAN_POINT('Ctrl Pts',(3.23444066545347,1.59180796310647,5.09654463903297));
#7747=CARTESIAN_POINT('Ctrl Pts',(3.34546820602455,-0.352083916784466,5.77101560163446));
#7748=CARTESIAN_POINT('Ctrl Pts',(3.45649574659563,-1.97428470703338,4.50529672953804));
#7749=CARTESIAN_POINT('Ctrl Pts',(3.5675232871667,-1.79269061716177,2.45573087208473));
#7750=CARTESIAN_POINT('Ctrl Pts',(3.67855082773778,0.0267936548760598,1.49493939893213));
#7751=CARTESIAN_POINT('Ctrl Pts',(3.78957836830886,1.82179649485102,2.50072594871047));
#7752=CARTESIAN_POINT('Ctrl Pts',(3.90060590887995,1.9523202444135,4.55416710996289));
#7753=CARTESIAN_POINT('Ctrl Pts',(4.01163344945101,0.299111035420234,5.77913573698043));
#7754=CARTESIAN_POINT('Ctrl Pts',(4.12266099002211,-1.62738002173627,5.05644524881745));
#7755=CARTESIAN_POINT('Ctrl Pts',(4.23368853059317,-2.06701946096996,3.04637846975065));
#7756=CARTESIAN_POINT('Ctrl Pts',(4.34471607116426,-0.618131624590583,1.58542875397713));
#7757=CARTESIAN_POINT('Ctrl Pts',(4.45574361173533,1.39551060095016,2.00838874861888));
#7758=CARTESIAN_POINT('Ctrl Pts',(4.56677115230641,2.13414805541207,3.92882237031159));
#7759=CARTESIAN_POINT('Ctrl Pts',(4.67779869287749,0.92292637523073,5.59212998197178));
#7760=CARTESIAN_POINT('Ctrl Pts',(4.78882623344857,-1.13152462500531,5.47863495099715));
#7761=CARTESIAN_POINT('Ctrl Pts',(4.89985377401965,-2.15216109701436,3.69203133383899));
#7762=CARTESIAN_POINT('Ctrl Pts',(5.01088131459073,-1.2064806349059,1.86464582482029));
#7763=CARTESIAN_POINT('Ctrl Pts',(5.1219088551618,0.841497345636436,1.66606330521921));
#7764=CARTESIAN_POINT('Ctrl Pts',(5.23293639573289,2.12064437238283,3.27772081718985));
#7765=CARTESIAN_POINT('Ctrl Pts',(5.34396393630396,1.46226796976159,5.22712644242662));
#7766=CARTESIAN_POINT('Ctrl Pts',(5.45499147687504,-0.532102198828669,5.73322021013476));
#7767=CARTESIAN_POINT('Ctrl Pts',(5.56601901744612,-2.04032571197971,4.33359224103263));
#7768=CARTESIAN_POINT('Ctrl Pts',(5.6770465580172,-1.68439684099265,2.30704485548668));
#7769=CARTESIAN_POINT('Ctrl Pts',(5.78807409858828,0.210450406220844,1.50505942555297));
#7770=CARTESIAN_POINT('Ctrl Pts',(5.89910163915935,1.91307136502743,2.66049992560517));
#7771=CARTESIAN_POINT('Ctrl Pts',(6.01012917973044,1.86772094212562,4.71744722891832));
#7772=CARTESIAN_POINT('Ctrl Pts',(6.1211567203015,0.116121264772982,5.79706453592731));
#7773=CARTESIAN_POINT('Ctrl Pts',(6.2321842608726,-1.74193664512735,4.9120235296154));
#7774=CARTESIAN_POINT('Ctrl Pts',(6.34321180144366,-2.00777602762851,2.87274675403155));
#7775=CARTESIAN_POINT('Ctrl Pts',(6.45423934201476,-0.440583748475745,1.53892016467367));
#7776=CARTESIAN_POINT('Ctrl Pts',(6.56526688258582,1.53193716163296,2.13609130675508));
#7777=CARTESIAN_POINT('Ctrl Pts',(6.63928524296654,1.90934849916403,3.44784970607045));
#7778=CARTESIAN_POINT('Ctrl Pts',(6.6762944231569,1.77928703864022,4.03891751659649));
#7779=CARTESIAN_POINT('Ctrl Pts',(2.42387384126203,0.979727419285334,2.27368025078364));
#7780=CARTESIAN_POINT('Ctrl Pts',(2.46089489447305,1.43622363149362,2.59923419867212));
#7781=CARTESIAN_POINT('Ctrl Pts',(2.53492512787443,1.99115683342641,3.73540524587877));
#7782=CARTESIAN_POINT('Ctrl Pts',(2.64596454146616,1.00567667700427,5.37027542442224));
#7783=CARTESIAN_POINT('Ctrl Pts',(2.75699208203724,-0.899465872904321,5.42597405909269));
#7784=CARTESIAN_POINT('Ctrl Pts',(2.86801962260832,-1.98232364567101,3.85911121162473));
#7785=CARTESIAN_POINT('Ctrl Pts',(2.9790471631794,-1.25429163898582,2.09756028172128));
#7786=CARTESIAN_POINT('Ctrl Pts',(3.09007470375048,0.619853644373857,1.75266217331931));
#7787=CARTESIAN_POINT('Ctrl Pts',(3.20110224432155,1.9276020995976,3.13854330669838));
#7788=CARTESIAN_POINT('Ctrl Pts',(3.31212978489263,1.47423759301864,4.98951092275774));
#7789=CARTESIAN_POINT('Ctrl Pts',(3.42315732546371,-0.326079123896298,5.61416569991195));
#7790=CARTESIAN_POINT('Ctrl Pts',(3.53418486603479,-1.82846474065272,4.44193237360281));
#7791=CARTESIAN_POINT('Ctrl Pts',(3.64521240660587,-1.66028312568185,2.54374672152922));
#7792=CARTESIAN_POINT('Ctrl Pts',(3.75623994717695,0.0248146850550797,1.65391896491398));
#7793=CARTESIAN_POINT('Ctrl Pts',(3.86726748774802,1.6872392535954,2.58541847779621));
#7794=CARTESIAN_POINT('Ctrl Pts',(3.97829502831911,1.8081225654311,4.4871932051084));
#7795=CARTESIAN_POINT('Ctrl Pts',(4.08932256889018,0.277018800711796,5.6216860849489));
#7796=CARTESIAN_POINT('Ctrl Pts',(4.20035010946126,-1.50718231204793,4.95237325924367));
#7797=CARTESIAN_POINT('Ctrl Pts',(4.31137765003234,-1.9143501386412,3.09076929767336));
#7798=CARTESIAN_POINT('Ctrl Pts',(4.42240519060342,-0.572476642613814,1.73772480837452));
#7799=CARTESIAN_POINT('Ctrl Pts',(4.5334327311745,1.29243868422536,2.12944512822199));
#7800=CARTESIAN_POINT('Ctrl Pts',(4.64446027174558,1.97652063896961,3.90803620554717));
#7801=CARTESIAN_POINT('Ctrl Pts',(4.75548781231665,0.85475936136058,5.44849250850354));
#7802=CARTESIAN_POINT('Ctrl Pts',(4.86651535288773,-1.04795061858702,5.34338018015643));
#7803=CARTESIAN_POINT('Ctrl Pts',(4.97754289345882,-1.99320324372482,3.68873447082252));
#7804=CARTESIAN_POINT('Ctrl Pts',(5.08857043402989,-1.11737040425166,1.99631900565835));
#7805=CARTESIAN_POINT('Ctrl Pts',(5.19959797460097,0.779344650934923,1.81240372033652));
#7806=CARTESIAN_POINT('Ctrl Pts',(5.31062551517205,1.96401433316682,3.305024781599));
#7807=CARTESIAN_POINT('Ctrl Pts',(5.42165305574313,1.35426537751614,5.11044800058928));
#7808=CARTESIAN_POINT('Ctrl Pts',(5.53268059631421,-0.492801319645516,5.5791618625879));
#7809=CARTESIAN_POINT('Ctrl Pts',(5.64370813688528,-1.88962798045874,4.2829099175581));
#7810=CARTESIAN_POINT('Ctrl Pts',(5.75473567745637,-1.55998788930993,2.40604260124246));
#7811=CARTESIAN_POINT('Ctrl Pts',(5.86576321802744,0.194906614056222,1.66329152996741));
#7812=CARTESIAN_POINT('Ctrl Pts',(5.97679075859853,1.77177259431909,2.73339160557513));
#7813=CARTESIAN_POINT('Ctrl Pts',(6.08781829916959,1.72977173752561,4.63841351254227));
#7814=CARTESIAN_POINT('Ctrl Pts',(6.19884583974068,0.107544589451052,5.63829066918126));
#7815=CARTESIAN_POINT('Ctrl Pts',(6.30987338031176,-1.61327782397314,4.81861847686368));
#7816=CARTESIAN_POINT('Ctrl Pts',(6.42090092088283,-1.85948240421864,2.92996195873161));
#7817=CARTESIAN_POINT('Ctrl Pts',(6.53192846145392,-0.408042389490527,1.69465132693797));
#7818=CARTESIAN_POINT('Ctrl Pts',(6.642956002025,1.41878882765114,2.2477156208269));
#7819=CARTESIAN_POINT('Ctrl Pts',(6.71697436240571,1.76832469800446,3.46258801124687));
#7820=CARTESIAN_POINT('Ctrl Pts',(6.75398354259607,1.64786953070343,4.00999976347872));
#7821=CARTESIAN_POINT('Ctrl Pts',(2.5015629607012,0.901594209403805,2.38323388698939));
#7822=CARTESIAN_POINT('Ctrl Pts',(2.53858401391222,1.3216848728273,2.68282492474856));
#7823=CARTESIAN_POINT('Ctrl Pts',(2.6126142473136,1.83236218124995,3.72838639101944));
#7824=CARTESIAN_POINT('Ctrl Pts',(2.72365366090533,0.925474015191809,5.23287575927348));
#7825=CARTESIAN_POINT('Ctrl Pts',(2.83468120147641,-0.827733517102571,5.28413243077424));
#7826=CARTESIAN_POINT('Ctrl Pts',(2.94570874204748,-1.82423343975097,3.84222681253854));
#7827=CARTESIAN_POINT('Ctrl Pts',(3.05673628261856,-1.15426194710171,2.22115947614681));
#7828=CARTESIAN_POINT('Ctrl Pts',(3.16776382318964,0.570420349011948,1.9037669736522));
#7829=CARTESIAN_POINT('Ctrl Pts',(3.27879136376072,1.77387593408332,3.17912415992756));
#7830=CARTESIAN_POINT('Ctrl Pts',(3.3898189043318,1.35666722293081,4.88247720648249));
#7831=CARTESIAN_POINT('Ctrl Pts',(3.50084644490287,-0.300074331008131,5.45731579818944));
#7832=CARTESIAN_POINT('Ctrl Pts',(3.61187398547396,-1.68264477427207,4.37856801766755));
#7833=CARTESIAN_POINT('Ctrl Pts',(3.72290152604503,-1.52787563420194,2.6317625709737));
#7834=CARTESIAN_POINT('Ctrl Pts',(3.83392906661612,0.0228357152340999,1.81289853089582));
#7835=CARTESIAN_POINT('Ctrl Pts',(3.94495660718719,1.55268201233977,2.67011100688194));
#7836=CARTESIAN_POINT('Ctrl Pts',(4.05598414775828,1.66392488644871,4.42021930025391));
#7837=CARTESIAN_POINT('Ctrl Pts',(4.16701168832934,0.254926566003358,5.46423643291735));
#7838=CARTESIAN_POINT('Ctrl Pts',(4.27803922890044,-1.38698460235959,4.84830126966989));
#7839=CARTESIAN_POINT('Ctrl Pts',(4.3890667694715,-1.76168081631245,3.13516012559607));
#7840=CARTESIAN_POINT('Ctrl Pts',(4.50009431004259,-0.526821660637044,1.8900208627719));
#7841=CARTESIAN_POINT('Ctrl Pts',(4.61112185061366,1.18936676750055,2.25050150782511));
#7842=CARTESIAN_POINT('Ctrl Pts',(4.72214939118474,1.81889322252715,3.88725004078275));
#7843=CARTESIAN_POINT('Ctrl Pts',(4.83317693175582,0.78659234749043,5.30485503503531));
#7844=CARTESIAN_POINT('Ctrl Pts',(4.9442044723269,-0.964376612168717,5.2081254093157));
#7845=CARTESIAN_POINT('Ctrl Pts',(5.05523201289798,-1.83424539043528,3.68543760780607));
#7846=CARTESIAN_POINT('Ctrl Pts',(5.16625955346906,-1.02826017359741,2.12799218649641));
#7847=CARTESIAN_POINT('Ctrl Pts',(5.27728709404013,0.717191956233405,1.95874413545384));
#7848=CARTESIAN_POINT('Ctrl Pts',(5.38831463461122,1.80738429395082,3.33232874600814));
#7849=CARTESIAN_POINT('Ctrl Pts',(5.49934217518229,1.2462627852707,4.99376955875193));
#7850=CARTESIAN_POINT('Ctrl Pts',(5.61036971575337,-0.45350044046236,5.42510351504104));
#7851=CARTESIAN_POINT('Ctrl Pts',(5.72139725632445,-1.73893024893777,4.23222759408355));
#7852=CARTESIAN_POINT('Ctrl Pts',(5.83242479689554,-1.43557893762722,2.50504034699825));
#7853=CARTESIAN_POINT('Ctrl Pts',(5.94345233746659,0.179362821891601,1.82152363438183));
#7854=CARTESIAN_POINT('Ctrl Pts',(6.0544798780377,1.63047382361075,2.80628328554509));
#7855=CARTESIAN_POINT('Ctrl Pts',(6.16550741860875,1.59182253292561,4.55937979616623));
#7856=CARTESIAN_POINT('Ctrl Pts',(6.27653495917986,0.0989679141291208,5.47951680243522));
#7857=CARTESIAN_POINT('Ctrl Pts',(6.38756249975091,-1.48461900281893,4.72521342411197));
#7858=CARTESIAN_POINT('Ctrl Pts',(6.498590040322,-1.71118878080877,2.98717716343168));
#7859=CARTESIAN_POINT('Ctrl Pts',(6.60961758089308,-0.375501030505309,1.85038248920226));
#7860=CARTESIAN_POINT('Ctrl Pts',(6.72064512146415,1.30564049366934,2.35933993489874));
#7861=CARTESIAN_POINT('Ctrl Pts',(6.79466348184488,1.62730089684488,3.47732631642329));
#7862=CARTESIAN_POINT('Ctrl Pts',(6.83167266203525,1.51645202276663,3.98108201036094));
#7863=CARTESIAN_POINT('Ctrl Pts',(6.6,-0.426653165344755,2.14890699090199));
#7864=CARTESIAN_POINT('Ctrl Pts',(6.6,-0.392021497824994,2.13398863376564));
#7865=CARTESIAN_POINT('Ctrl Pts',(6.6,-0.356894299772028,2.12044962477061));
#7866=CARTESIAN_POINT('Ctrl Pts',(6.6,-0.32133619505273,2.10833833927896));
#7867=CARTESIAN_POINT('Ctrl Pts',(6.6,-0.265498001506515,2.08931954430338));
#7868=CARTESIAN_POINT('Ctrl Pts',(6.6,-0.208598730002439,2.07381868407842));
#7869=CARTESIAN_POINT('Ctrl Pts',(6.6,-0.150939387672386,2.06168379970761));
#7870=CARTESIAN_POINT('Ctrl Pts',(6.6,-0.0913824051006462,2.0491495412895));
#7871=CARTESIAN_POINT('Ctrl Pts',(6.6,-0.031013775489611,2.04020620059287));
#7872=CARTESIAN_POINT('Ctrl Pts',(6.6,0.0298636687991222,2.03473391298628));
#7873=CARTESIAN_POINT('Ctrl Pts',(6.6,0.0578342379090375,2.0322196320325));
#7874=CARTESIAN_POINT('Ctrl Pts',(6.6,0.0859125425023256,2.03043876497452));
#7875=CARTESIAN_POINT('Ctrl Pts',(6.6,0.114070466778614,2.02938311428739));
#7876=CARTESIAN_POINT('Ctrl Pts',(6.6,0.127825777648026,2.02886742274605));
#7877=CARTESIAN_POINT('Ctrl Pts',(6.6,0.141600097379563,2.02852482806017));
#7878=CARTESIAN_POINT('Ctrl Pts',(6.6,0.15539018623994,2.02835456195391));
#7879=CARTESIAN_POINT('Ctrl Pts',(6.6,0.16829253625044,2.02819525675146));
#7880=CARTESIAN_POINT('Ctrl Pts',(6.6,0.181210508110224,2.02818695541741));
#7881=CARTESIAN_POINT('Ctrl Pts',(6.6,0.194119545976811,2.02832850350873));
#7882=CARTESIAN_POINT('Ctrl Pts',(6.6,0.257354815079917,2.02902188064017));
#7883=CARTESIAN_POINT('Ctrl Pts',(6.6,0.320489102895611,2.03330438411646));
#7884=CARTESIAN_POINT('Ctrl Pts',(6.6,0.383193278384661,2.04101811063467));
#7885=CARTESIAN_POINT('Ctrl Pts',(6.6,0.447605187382698,2.04894191868496));
#7886=CARTESIAN_POINT('Ctrl Pts',(6.6,0.511564220195584,2.06048621348128));
#7887=CARTESIAN_POINT('Ctrl Pts',(6.6,0.574732782147204,2.07553202138906));
#7888=CARTESIAN_POINT('Ctrl Pts',(6.6,0.636493843821096,2.09024258375453));
#7889=CARTESIAN_POINT('Ctrl Pts',(6.6,0.697500338542476,2.10830059516598));
#7890=CARTESIAN_POINT('Ctrl Pts',(6.6,0.757439278502091,2.1296429645003));
#7891=CARTESIAN_POINT('Ctrl Pts',(6.6,0.77025897939523,2.1342076563584));
#7892=CARTESIAN_POINT('Ctrl Pts',(6.6,0.783029821878101,2.13892276046386));
#7893=CARTESIAN_POINT('Ctrl Pts',(6.6,0.795748687204425,2.14378793840273));
#7894=CARTESIAN_POINT('Ctrl Pts',(6.6,0.80498703879146,2.14732176183585));
#7895=CARTESIAN_POINT('Ctrl Pts',(6.6,0.814196614693253,2.15093430581471));
#7896=CARTESIAN_POINT('Ctrl Pts',(6.6,0.823367217856443,2.15462160067646));
#7897=CARTESIAN_POINT('Ctrl Pts',(6.6,0.885585028569377,2.17963799378264));
#7898=CARTESIAN_POINT('Ctrl Pts',(6.6,0.946123260308849,2.20813435132922));
#7899=CARTESIAN_POINT('Ctrl Pts',(6.6,1.00463249771459,2.23997375815824));
#7900=CARTESIAN_POINT('Ctrl Pts',(6.6,1.06301708518201,2.27174533330335));
#7901=CARTESIAN_POINT('Ctrl Pts',(6.6,1.11938248640286,2.30684585706902));
#7902=CARTESIAN_POINT('Ctrl Pts',(6.6,1.17337908236605,2.34519025244813));
#7903=CARTESIAN_POINT('Ctrl Pts',(6.6,1.20112489863409,2.36489328242844));
#7904=CARTESIAN_POINT('Ctrl Pts',(6.6,1.22824511880884,2.38545362366961));
#7905=CARTESIAN_POINT('Ctrl Pts',(6.6,1.25469050295843,2.40686481674482));
#7906=CARTESIAN_POINT('Ctrl Pts',(6.6,1.28458305880661,2.43106697169013));
#7907=CARTESIAN_POINT('Ctrl Pts',(6.6,1.31361349719728,2.45635617344964));
#7908=CARTESIAN_POINT('Ctrl Pts',(6.6,1.34176728722325,2.48267337167383));
#7909=CARTESIAN_POINT('Ctrl Pts',(6.6,1.35578764887621,2.49577912533809));
#7910=CARTESIAN_POINT('Ctrl Pts',(6.6,1.3695970620793,2.50914671196291));
#7911=CARTESIAN_POINT('Ctrl Pts',(6.6,1.38316141179628,2.52273642352609));
#7912=CARTESIAN_POINT('Ctrl Pts',(6.6,1.42965922152231,2.56932117220041));
#7913=CARTESIAN_POINT('Ctrl Pts',(6.6,1.47332647655611,2.6185511247577));
#7914=CARTESIAN_POINT('Ctrl Pts',(6.6,1.51413239558925,2.67007175656389));
#7915=CARTESIAN_POINT('Ctrl Pts',(6.6,1.55582152221007,2.72270750632383));
#7916=CARTESIAN_POINT('Ctrl Pts',(6.6,1.59452464031864,2.7777347408237));
#7917=CARTESIAN_POINT('Ctrl Pts',(6.6,1.63018231428798,2.83482333659135));
#7918=CARTESIAN_POINT('Ctrl Pts',(6.6,1.66654200783675,2.89303587869451));
#7919=CARTESIAN_POINT('Ctrl Pts',(6.6,1.69973577324958,2.95339246282403));
#7920=CARTESIAN_POINT('Ctrl Pts',(6.6,1.72966447542417,3.01558249180135));
#7921=CARTESIAN_POINT('Ctrl Pts',(6.6,1.73401928737242,3.02463152706096));
#7922=CARTESIAN_POINT('Ctrl Pts',(6.6,1.73830490042804,3.03371943563744));
#7923=CARTESIAN_POINT('Ctrl Pts',(6.6,1.74252093471433,3.04284531379462));
#7924=CARTESIAN_POINT('Ctrl Pts',(6.6,1.74801629838275,3.05474038291927));
#7925=CARTESIAN_POINT('Ctrl Pts',(6.6,1.75339345222138,3.06669996012485));
#7926=CARTESIAN_POINT('Ctrl Pts',(6.6,1.75865150293071,3.07872207211292));
#7927=CARTESIAN_POINT('Ctrl Pts',(6.6,1.76360055612823,3.09003768602855));
#7928=CARTESIAN_POINT('Ctrl Pts',(6.6,1.76844015485371,3.1013997152548));
#7929=CARTESIAN_POINT('Ctrl Pts',(6.6,1.77316959011757,3.11280520801871));
#7930=CARTESIAN_POINT('Ctrl Pts',(6.6,1.80041932406339,3.17852058966537));
#7931=CARTESIAN_POINT('Ctrl Pts',(6.6,1.82401955598892,3.24568623982158));
#7932=CARTESIAN_POINT('Ctrl Pts',(6.6,1.84389319791717,3.31394437453886));
#7933=CARTESIAN_POINT('Ctrl Pts',(6.6,1.86154775129936,3.37458081387317));
#7934=CARTESIAN_POINT('Ctrl Pts',(6.6,1.87626122908549,3.43608043797506));
#7935=CARTESIAN_POINT('Ctrl Pts',(6.6,1.88795171173133,3.49821270271176));
#7936=CARTESIAN_POINT('Ctrl Pts',(6.6,1.89137817487732,3.51642357746748));
#7937=CARTESIAN_POINT('Ctrl Pts',(6.6,1.89454475423252,3.5346888947779));
#7938=CARTESIAN_POINT('Ctrl Pts',(6.6,1.89744890221981,3.55300305386885));
#7939=CARTESIAN_POINT('Ctrl Pts',(6.6,1.89980101603368,3.5678359710534));
#7940=CARTESIAN_POINT('Ctrl Pts',(6.6,1.90197972572745,3.58269332812843));
#7941=CARTESIAN_POINT('Ctrl Pts',(6.6,1.9039834114727,3.59756590193512));
#7942=CARTESIAN_POINT('Ctrl Pts',(6.6,1.91367106629442,3.66947356594452));
#7943=CARTESIAN_POINT('Ctrl Pts',(6.6,1.91927795233095,3.74177918255773));
#7944=CARTESIAN_POINT('Ctrl Pts',(6.6,1.92070287200251,3.81413426669386));
#7945=CARTESIAN_POINT('Ctrl Pts',(6.6,1.92211579885107,3.8858803749454));
#7946=CARTESIAN_POINT('Ctrl Pts',(6.6,1.91941728760809,3.95767611431338));
#7947=CARTESIAN_POINT('Ctrl Pts',(6.6,1.91246071929237,4.02919789218586));
#7948=CARTESIAN_POINT('Ctrl Pts',(6.6,1.91122396329219,4.0419132115665));
#7949=CARTESIAN_POINT('Ctrl Pts',(6.6,1.9098524915949,4.05461989137718));
#7950=CARTESIAN_POINT('Ctrl Pts',(6.6,1.90834530359594,4.06731613031539));
#7951=CARTESIAN_POINT('Ctrl Pts',(2.5,0.863580915426621,5.40376507534352));
#7952=CARTESIAN_POINT('Ctrl Pts',(2.5,0.903481800679317,5.37926660921982));
#7953=CARTESIAN_POINT('Ctrl Pts',(2.5,0.942351921741602,5.35328747129858));
#7954=CARTESIAN_POINT('Ctrl Pts',(2.5,0.98009997800088,5.32582783981609));
#7955=CARTESIAN_POINT('Ctrl Pts',(2.5,1.03756562079836,5.28402475031965));
#7956=CARTESIAN_POINT('Ctrl Pts',(2.5,1.09243293237426,5.23879201435724));
#7957=CARTESIAN_POINT('Ctrl Pts',(2.5,1.14456529515591,5.19047296275182));
#7958=CARTESIAN_POINT('Ctrl Pts',(2.5,1.19725087194605,5.14164116292633));
#7959=CARTESIAN_POINT('Ctrl Pts',(2.5,1.2471436239525,5.08965615147515));
#7960=CARTESIAN_POINT('Ctrl Pts',(2.5,1.29405766001486,5.03484467912125));
#7961=CARTESIAN_POINT('Ctrl Pts',(2.5,1.32834049376268,4.99479072614897));
#7962=CARTESIAN_POINT('Ctrl Pts',(2.49999999999999,1.36103175781229,4.95322678141866));
#7963=CARTESIAN_POINT('Ctrl Pts',(2.5,1.39204180474702,4.91027607043137));
#7964=CARTESIAN_POINT('Ctrl Pts',(2.5,1.39932292818565,4.9001912927742));
#7965=CARTESIAN_POINT('Ctrl Pts',(2.5,1.40651184414629,4.89002911337057));
#7966=CARTESIAN_POINT('Ctrl Pts',(2.5,1.41359773403284,4.87980534663974));
#7967=CARTESIAN_POINT('Ctrl Pts',(2.5,1.4537289806095,4.82190259762929));
#7968=CARTESIAN_POINT('Ctrl Pts',(2.5,1.49063491990531,4.76192357977479));
#7969=CARTESIAN_POINT('Ctrl Pts',(2.5,1.5241744546024,4.70019324897602));
#7970=CARTESIAN_POINT('Ctrl Pts',(2.5,1.55724799453256,4.63932059289972));
#7971=CARTESIAN_POINT('Ctrl Pts',(2.5,1.58704824368533,4.57674389634121));
#7972=CARTESIAN_POINT('Ctrl Pts',(2.5,1.61339223682867,4.51276105655928));
#7973=CARTESIAN_POINT('Ctrl Pts',(2.5,1.63919258494756,4.45009859187415));
#7974=CARTESIAN_POINT('Ctrl Pts',(2.5,1.66167798030882,4.38608652278053));
#7975=CARTESIAN_POINT('Ctrl Pts',(2.5,1.68062808017528,4.32100573103691));
#7976=CARTESIAN_POINT('Ctrl Pts',(2.5,1.68520397395649,4.30529062703671));
#7977=CARTESIAN_POINT('Ctrl Pts',(2.5,1.68957350060244,4.28951324697453));
#7978=CARTESIAN_POINT('Ctrl Pts',(2.5,1.69373310938903,4.27367764327361));
#7979=CARTESIAN_POINT('Ctrl Pts',(2.5,1.69762827690034,4.25884876579445));
#7980=CARTESIAN_POINT('Ctrl Pts',(2.5,1.70134027318467,4.24396443866154));
#7981=CARTESIAN_POINT('Ctrl Pts',(2.5,1.70485982262735,4.22905603382341));
#7982=CARTESIAN_POINT('Ctrl Pts',(2.5,1.72026850374741,4.16378664070909));
#7983=CARTESIAN_POINT('Ctrl Pts',(2.5,1.73201964293855,4.09796147516516));
#7984=CARTESIAN_POINT('Ctrl Pts',(2.5,1.73995104778607,4.03185909017483));
#7985=CARTESIAN_POINT('Ctrl Pts',(2.5,1.74764478811446,3.96773746292473));
#7986=CARTESIAN_POINT('Ctrl Pts',(2.5,1.75174426392432,3.90335417483549));
#7987=CARTESIAN_POINT('Ctrl Pts',(2.5,1.75205333162734,3.83896894622148));
#7988=CARTESIAN_POINT('Ctrl Pts',(2.5,1.75223292383878,3.80155615453449));
#7989=CARTESIAN_POINT('Ctrl Pts',(2.5,1.75113178109454,3.76414287274798));
#7990=CARTESIAN_POINT('Ctrl Pts',(2.5,1.7487036258443,3.72678250885966));
#7991=CARTESIAN_POINT('Ctrl Pts',(2.5,1.74647840079726,3.69254449319611));
#7992=CARTESIAN_POINT('Ctrl Pts',(2.5,1.74313852381005,3.65835091190104));
#7993=CARTESIAN_POINT('Ctrl Pts',(2.5,1.73870317030216,3.62424537115788));
#7994=CARTESIAN_POINT('Ctrl Pts',(2.5,1.73685252518352,3.61001488143867));
#7995=CARTESIAN_POINT('Ctrl Pts',(2.5,1.73481112807425,3.59579974532583));
#7996=CARTESIAN_POINT('Ctrl Pts',(2.5,1.73258023476543,3.58160325113988));
#7997=CARTESIAN_POINT('Ctrl Pts',(2.5,1.73102147713734,3.57168395400586));
#7998=CARTESIAN_POINT('Ctrl Pts',(2.5,1.7293705537313,3.56177631081533));
#7999=CARTESIAN_POINT('Ctrl Pts',(2.5,1.72762964038082,3.55188979175844));
#8000=CARTESIAN_POINT('Ctrl Pts',(2.5,1.71639361008828,3.48808120095145));
#8001=CARTESIAN_POINT('Ctrl Pts',(2.5,1.7013973068787,3.42504861484961));
#8002=CARTESIAN_POINT('Ctrl Pts',(2.5,1.68284183603963,3.36305994407503));
#8003=CARTESIAN_POINT('Ctrl Pts',(2.5,1.663527963892,3.29853766531827));
#8004=CARTESIAN_POINT('Ctrl Pts',(2.5,1.64035754708482,3.23514519508613));
#8005=CARTESIAN_POINT('Ctrl Pts',(2.5,1.61350667224645,3.17321353421575));
#8006=CARTESIAN_POINT('Ctrl Pts',(2.5,1.59336851611767,3.12676478856296));
#8007=CARTESIAN_POINT('Ctrl Pts',(2.5,1.57115896484118,3.08113825840607));
#8008=CARTESIAN_POINT('Ctrl Pts',(2.5,1.54693754647141,3.03648971833169));
#8009=CARTESIAN_POINT('Ctrl Pts',(2.5,1.53615118929738,3.01660669194615));
#8010=CARTESIAN_POINT('Ctrl Pts',(2.5,1.52496597272822,2.99691826608897));
#8011=CARTESIAN_POINT('Ctrl Pts',(2.5,1.51338567219742,2.97743787138593));
#8012=CARTESIAN_POINT('Ctrl Pts',(2.5,1.50517306502384,2.96362261427262));
#8013=CARTESIAN_POINT('Ctrl Pts',(2.5,1.49676293575689,2.94991442666182));
#8014=CARTESIAN_POINT('Ctrl Pts',(2.5,1.48816920216178,2.93633689673824));
#8015=CARTESIAN_POINT('Ctrl Pts',(2.5,1.45429941367692,2.88282487410349));
#8016=CARTESIAN_POINT('Ctrl Pts',(2.5,1.41753605926436,2.83126366672452));
#8017=CARTESIAN_POINT('Ctrl Pts',(2.5,1.37802108941853,2.7819436771186));
#8018=CARTESIAN_POINT('Ctrl Pts',(2.5,1.3464603183726,2.7425515959399));
#8019=CARTESIAN_POINT('Ctrl Pts',(2.5,1.31314338874534,2.70458976729865));
#8020=CARTESIAN_POINT('Ctrl Pts',(2.5,1.27813049929784,2.66822683678827));
#8021=CARTESIAN_POINT('Ctrl Pts',(2.5,1.26549763847306,2.65510687303871));
#8022=CARTESIAN_POINT('Ctrl Pts',(2.5,1.25264391284352,2.64219524937818));
#8023=CARTESIAN_POINT('Ctrl Pts',(2.5,1.23957189874079,2.62950057750473));
#8024=CARTESIAN_POINT('Ctrl Pts',(2.5,1.23011804990051,2.62031962742118));
#8025=CARTESIAN_POINT('Ctrl Pts',(2.5,1.22055629636979,2.61125828180273));
#8026=CARTESIAN_POINT('Ctrl Pts',(2.5,1.21089009782921,2.6023212812504));
#8027=CARTESIAN_POINT('Ctrl Pts',(2.5,1.16593824479605,2.56076050286386));
#8028=CARTESIAN_POINT('Ctrl Pts',(2.5,1.11871429572554,2.5218704031965));
#8029=CARTESIAN_POINT('Ctrl Pts',(2.5,1.06933638089496,2.48594621693982));
#8030=CARTESIAN_POINT('Ctrl Pts',(2.5,1.01995846606438,2.45002203068315));
#8031=CARTESIAN_POINT('Ctrl Pts',(2.5,0.968425945013954,2.41706310482043));
#8032=CARTESIAN_POINT('Ctrl Pts',(2.5,0.914840821524557,2.3874184035349));
#8033=CARTESIAN_POINT('Ctrl Pts',(2.5,0.911106104645141,2.38535225981689));
#8034=CARTESIAN_POINT('Ctrl Pts',(2.5,0.907361412733174,2.38330223944661));
#8035=CARTESIAN_POINT('Ctrl Pts',(2.5,0.903606778650209,2.38126847156104));
#8036=CARTESIAN_POINT('Origin',(6.6,0.,3.64739446828387));
#8037=CARTESIAN_POINT('',(6.6,-1.15470053837925,3.64739446828387));
#8038=CARTESIAN_POINT('',(6.6,-0.577350269189626,4.64739446828387));
#8039=CARTESIAN_POINT('',(6.6,-1.01036297108184,3.89739446828387));
#8040=CARTESIAN_POINT('',(6.6,0.577350269189627,4.64739446828387));
#8041=CARTESIAN_POINT('',(6.6,-0.288675134594813,4.64739446828387));
#8042=CARTESIAN_POINT('',(6.6,1.15470053837925,3.64739446828387));
#8043=CARTESIAN_POINT('',(6.6,0.721687836487033,4.39739446828387));
#8044=CARTESIAN_POINT('',(6.6,0.577350269189625,2.64739446828387));
#8045=CARTESIAN_POINT('',(6.6,1.01036297108184,3.39739446828387));
#8046=CARTESIAN_POINT('',(6.6,-0.577350269189626,2.64739446828387));
#8047=CARTESIAN_POINT('',(6.6,0.288675134594812,2.64739446828387));
#8048=CARTESIAN_POINT('',(6.6,-0.721687836487032,2.89739446828387));
#8049=CARTESIAN_POINT('Origin',(6.6,-1.15470053837925,3.64739446828387));
#8050=CARTESIAN_POINT('',(6.1,-1.15470053837925,3.64739446828387));
#8051=CARTESIAN_POINT('',(6.6,-1.15470053837925,3.64739446828387));
#8052=CARTESIAN_POINT('',(6.1,-0.577350269189626,4.64739446828387));
#8053=CARTESIAN_POINT('',(6.1,-0.577350269189626,4.64739446828387));
#8054=CARTESIAN_POINT('',(6.6,-0.577350269189626,4.64739446828387));
#8055=CARTESIAN_POINT('Origin',(6.6,-0.577350269189626,2.64739446828387));
#8056=CARTESIAN_POINT('',(6.1,-0.577350269189626,2.64739446828387));
#8057=CARTESIAN_POINT('',(6.6,-0.577350269189626,2.64739446828387));
#8058=CARTESIAN_POINT('',(6.1,-1.15470053837925,3.64739446828387));
#8059=CARTESIAN_POINT('Origin',(6.6,0.577350269189625,2.64739446828387));
#8060=CARTESIAN_POINT('',(6.1,0.577350269189625,2.64739446828387));
#8061=CARTESIAN_POINT('',(6.6,0.577350269189625,2.64739446828387));
#8062=CARTESIAN_POINT('',(6.1,-0.577350269189626,2.64739446828387));
#8063=CARTESIAN_POINT('Origin',(6.6,1.15470053837925,3.64739446828387));
#8064=CARTESIAN_POINT('',(6.1,1.15470053837925,3.64739446828387));
#8065=CARTESIAN_POINT('',(6.6,1.15470053837925,3.64739446828387));
#8066=CARTESIAN_POINT('',(6.1,0.577350269189625,2.64739446828387));
#8067=CARTESIAN_POINT('Origin',(6.6,0.577350269189627,4.64739446828387));
#8068=CARTESIAN_POINT('',(6.1,0.577350269189627,4.64739446828387));
#8069=CARTESIAN_POINT('',(6.6,0.577350269189627,4.64739446828387));
#8070=CARTESIAN_POINT('',(6.1,1.15470053837925,3.64739446828387));
#8071=CARTESIAN_POINT('Origin',(6.6,-0.577350269189626,4.64739446828387));
#8072=CARTESIAN_POINT('',(6.1,0.577350269189627,4.64739446828387));
#8073=CARTESIAN_POINT('Origin',(6.1,0.,3.64739446828387));
#8074=CARTESIAN_POINT('Origin',(2.5,0.,3.64739446828387));
#8075=CARTESIAN_POINT('',(0.,0.,0.));
#8076=CARTESIAN_POINT('Origin',(-2.67773308947627E-16,1.2059437743963,3.64739446828387));
#8077=CARTESIAN_POINT('',(1.55537930835193,3.0940562256037,3.64803845831604));
#8078=CARTESIAN_POINT('',(1.55549966270667,2.95594377439629,3.64841883122548));
#8079=CARTESIAN_POINT('',(1.5555,1.2059437743963,3.64739446828386));
#8080=CARTESIAN_POINT('',(0.903577229903434,2.50004392260581,2.38124738377906));
#8081=CARTESIAN_POINT('Ctrl Pts',(0.903577229903434,2.50004392260581,2.38124738377906));
#8082=CARTESIAN_POINT('Ctrl Pts',(0.85508552397506,2.50433411497395,2.34664160862681));
#8083=CARTESIAN_POINT('Ctrl Pts',(0.804491254712248,2.50862430734209,2.31474615079293));
#8084=CARTESIAN_POINT('Ctrl Pts',(0.752136324784236,2.51291449971023,2.28582508006303));
#8085=CARTESIAN_POINT('Ctrl Pts',(0.702087969422062,2.51701568125145,2.25817817026229));
#8086=CARTESIAN_POINT('Ctrl Pts',(0.650431357336846,2.52111686279267,2.2332493669833));
#8087=CARTESIAN_POINT('Ctrl Pts',(0.597496772224334,2.52521804433389,2.21122670051386));
#8088=CARTESIAN_POINT('Ctrl Pts',(0.544609525470966,2.52931555826907,2.18922372848223));
#8089=CARTESIAN_POINT('Ctrl Pts',(0.490447057473847,2.53341307220424,2.17012195018667));
#8090=CARTESIAN_POINT('Ctrl Pts',(0.435362908197919,2.53751058613941,2.15406282790205));
#8091=CARTESIAN_POINT('Ctrl Pts',(0.380305862575478,2.5416060839302,2.13801160736216));
#8092=CARTESIAN_POINT('Ctrl Pts',(0.324328543987183,2.54570158172099,2.12500022449484));
#8093=CARTESIAN_POINT('Ctrl Pts',(0.267800829156942,2.54979707951179,2.11512067881188));
#8094=CARTESIAN_POINT('Ctrl Pts',(0.211278192468849,2.55389220938536,2.10524202065352));
#8095=CARTESIAN_POINT('Ctrl Pts',(0.154205781558203,2.55798733925892,2.09849473034023));
#8096=CARTESIAN_POINT('Ctrl Pts',(0.0969625372345533,2.56208246913249,2.09491950347025));
#8097=CARTESIAN_POINT('Ctrl Pts',(0.0396642560698652,2.56618153629184,2.09134083917819));
#8098=CARTESIAN_POINT('Ctrl Pts',(-0.0178046547620221,2.57028060345119,
2.09094035559527));
#8099=CARTESIAN_POINT('Ctrl Pts',(-0.0750629135761472,2.57437967061054,
2.09370665890727));
#8100=CARTESIAN_POINT('Ctrl Pts',(-0.132353730100078,2.578481068547,2.0964745351714));
#8101=CARTESIAN_POINT('Ctrl Pts',(-0.189433127822198,2.58258246648346,2.10241272382604));
#8102=CARTESIAN_POINT('Ctrl Pts',(-0.245925895792534,2.58668386441992,2.11145804258825));
#8103=CARTESIAN_POINT('Ctrl Pts',(-0.302514885660697,2.5907922481053,2.12051876788423));
#8104=CARTESIAN_POINT('Ctrl Pts',(-0.358514735044354,2.59490063179069,2.13269706306549));
#8105=CARTESIAN_POINT('Ctrl Pts',(-0.413562868294952,2.59900901547607,2.14787921195346));
#8106=CARTESIAN_POINT('Ctrl Pts',(-0.43142604312879,2.60034219013111,2.15280583460031));
#8107=CARTESIAN_POINT('Ctrl Pts',(-0.449189147593431,2.60167536478614,2.15804838267405));
#8108=CARTESIAN_POINT('Ctrl Pts',(-0.46684025607362,2.60300853944117,2.16360188665087));
#8109=CARTESIAN_POINT('Ctrl Pts',(-0.521858625278674,2.60716403457439,2.18091211578018));
#8110=CARTESIAN_POINT('Ctrl Pts',(-0.576023644694715,2.61131952970761,2.20132138484263));
#8111=CARTESIAN_POINT('Ctrl Pts',(-0.628963033455794,2.61547502484083,2.22472593607193));
#8112=CARTESIAN_POINT('Ctrl Pts',(-0.681811493753012,2.61962338251369,2.24809028774584));
#8113=CARTESIAN_POINT('Ctrl Pts',(-0.73343803157307,2.62377174018655,2.27443950101458));
#8114=CARTESIAN_POINT('Ctrl Pts',(-0.783487045040432,2.6279200978594,2.30362056607643));
#8115=CARTESIAN_POINT('Ctrl Pts',(-0.833488047437585,2.63206447609135,2.33277363829554));
#8116=CARTESIAN_POINT('Ctrl Pts',(-0.881914078343796,2.6362088543233,2.36475291915533));
#8117=CARTESIAN_POINT('Ctrl Pts',(-0.928432591928929,2.64035323255525,2.39935874273587));
#8118=CARTESIAN_POINT('Ctrl Pts',(-0.974924175980665,2.64449521160968,2.43394453303052));
#8119=CARTESIAN_POINT('Ctrl Pts',(-1.0195100167281,2.64863719066411,2.47115354250067));
#8120=CARTESIAN_POINT('Ctrl Pts',(-1.06188696852167,2.65277916971855,2.51074310745072));
#8121=CARTESIAN_POINT('Ctrl Pts',(-1.10425550673426,2.6569203264185,2.55032481223158));
#8122=CARTESIAN_POINT('Ctrl Pts',(-1.14441564814527,2.66106148311845,2.59228577999225));
#8123=CARTESIAN_POINT('Ctrl Pts',(-1.18209939933821,2.6652026398184,2.63634488488836));
#8124=CARTESIAN_POINT('Ctrl Pts',(-1.2198180628967,2.66934763312091,2.68044480863946));
#8125=CARTESIAN_POINT('Ctrl Pts',(-1.25505541323189,2.67349262642343,2.72664635923883));
#8126=CARTESIAN_POINT('Ctrl Pts',(-1.28758315415599,2.67763761972594,2.7746345521937));
#8127=CARTESIAN_POINT('Ctrl Pts',(-1.32012488618734,2.68178439590806,2.82264338623632));
#8128=CARTESIAN_POINT('Ctrl Pts',(-1.3499544173738,2.68593117209018,2.87243994937997));
#8129=CARTESIAN_POINT('Ctrl Pts',(-1.37688806469825,2.6900779482723,2.92368215852846));
#8130=CARTESIAN_POINT('Ctrl Pts',(-1.40387406427022,2.69423278474608,2.97502396966493));
#8131=CARTESIAN_POINT('Ctrl Pts',(-1.42795271460863,2.69838762121987,3.02781656903583));
#8132=CARTESIAN_POINT('Ctrl Pts',(-1.44898778761461,2.70254245769366,3.08169610224088));
#8133=CARTESIAN_POINT('Ctrl Pts',(-1.46838439412369,2.70637366513319,3.13137884421063));
#8134=CARTESIAN_POINT('Ctrl Pts',(-1.48519355951164,2.71020487257272,3.18198527015832));
#8135=CARTESIAN_POINT('Ctrl Pts',(-1.49934664266485,2.71403608001225,3.23322071835562));
#8136=CARTESIAN_POINT('Ctrl Pts',(-1.51465181137774,2.71817915439409,3.28862682105783));
#8137=CARTESIAN_POINT('Ctrl Pts',(-1.52691450781882,2.72232222877592,3.34500138694105));
#8138=CARTESIAN_POINT('Ctrl Pts',(-1.5360179517072,2.72646530315776,3.40197828700557));
#8139=CARTESIAN_POINT('Ctrl Pts',(-1.54510497073757,2.73060090241158,3.45885238668986));
#8140=CARTESIAN_POINT('Ctrl Pts',(-1.55104396849636,2.73473650166541,3.51632615235849));
#8141=CARTESIAN_POINT('Ctrl Pts',(-1.55376848069946,2.73887210091923,3.57402036941438));
#8142=CARTESIAN_POINT('Ctrl Pts',(-1.55649024188075,2.74300352433428,3.63165633088644));
#8143=CARTESIAN_POINT('Ctrl Pts',(-1.55600392310557,2.74713494774932,3.68951178383784));
#8144=CARTESIAN_POINT('Ctrl Pts',(-1.55229470988028,2.75126637116436,3.74720119990903));
#8145=CARTESIAN_POINT('Ctrl Pts',(-1.54858780655053,2.75539522175441,3.80485469016077));
#8146=CARTESIAN_POINT('Ctrl Pts',(-1.54166202030053,2.75952407234446,3.86234182841598));
#8147=CARTESIAN_POINT('Ctrl Pts',(-1.53155460991275,2.76365292293451,3.91927813247688));
#8148=CARTESIAN_POINT('Ctrl Pts',(-1.52144958264269,2.76778080002723,3.97620101213824));
#8149=CARTESIAN_POINT('Ctrl Pts',(-1.50816451151996,2.77190867711994,4.03257280145901));
#8150=CARTESIAN_POINT('Ctrl Pts',(-1.49178807918711,2.77603655421266,4.08801741003253));
#8151=CARTESIAN_POINT('Ctrl Pts',(-1.47539694624562,2.78016813677092,4.14351178948869));
#8152=CARTESIAN_POINT('Ctrl Pts',(-1.45590905346099,2.78429971932918,4.19807682245725));
#8153=CARTESIAN_POINT('Ctrl Pts',(-1.4334631269432,2.78843130188743,4.25135118336719));
#8154=CARTESIAN_POINT('Ctrl Pts',(-1.41100802357335,2.79256457361285,4.30464732510796));
#8155=CARTESIAN_POINT('Ctrl Pts',(-1.38559270429132,2.79669784533826,4.35665127207841));
#8156=CARTESIAN_POINT('Ctrl Pts',(-1.35740294273004,2.80083111706367,4.40702431305554));
#8157=CARTESIAN_POINT('Ctrl Pts',(-1.32915808863627,2.80497246662991,4.45749580035656));
#8158=CARTESIAN_POINT('Ctrl Pts',(-1.29812823699444,2.80911381619615,4.50632956924819));
#8159=CARTESIAN_POINT('Ctrl Pts',(-1.26454328228958,2.81325516576239,4.55321483525312));
#8160=CARTESIAN_POINT('Ctrl Pts',(-1.23262241414806,2.81719131736937,4.59777700325588));
#8161=CARTESIAN_POINT('Ctrl Pts',(-1.19839396464653,2.82112746897635,4.64057893014162));
#8162=CARTESIAN_POINT('Ctrl Pts',(-1.16208710892346,2.82506362058333,4.68138373383449));
#8163=CARTESIAN_POINT('Ctrl Pts',(-1.12381204372855,2.82921315257595,4.72440058259503));
#8164=CARTESIAN_POINT('Ctrl Pts',(-1.0830653595052,2.83336268456856,4.7653790955833));
#8165=CARTESIAN_POINT('Ctrl Pts',(-1.04009256905409,2.83751221656118,4.80402219482274));
#8166=CARTESIAN_POINT('Ctrl Pts',(-0.997195985606611,2.84165438986481,4.84259676523792));
#8167=CARTESIAN_POINT('Ctrl Pts',(-0.952081515568061,2.84579656316844,4.87884379743944));
#8168=CARTESIAN_POINT('Ctrl Pts',(-0.905032885213852,2.84993873647208,4.91250147035187));
#8169=CARTESIAN_POINT('Ctrl Pts',(-0.858030931578233,2.85407680034561,4.94612575164982));
#8170=CARTESIAN_POINT('Ctrl Pts',(-0.80909904069553,2.85821486421915,4.97716546230243));
#8171=CARTESIAN_POINT('Ctrl Pts',(-0.758554187283879,2.86235292809268,5.00539881104353));
#8172=CARTESIAN_POINT('Ctrl Pts',(-0.708040087859642,2.8664884741636,5.03361498121959));
#8173=CARTESIAN_POINT('Ctrl Pts',(-0.655915424773617,2.87062402023451,5.05902792115146));
#8174=CARTESIAN_POINT('Ctrl Pts',(-0.602524480517743,2.87475956630543,5.08146019215319));
#8175=CARTESIAN_POINT('Ctrl Pts',(-0.549145539849393,2.87889418260464,5.10388741983283));
#8176=CARTESIAN_POINT('Ctrl Pts',(-0.49450136273391,2.88302879890385,5.12333510754783));
#8177=CARTESIAN_POINT('Ctrl Pts',(-0.438957034282652,2.88716341520306,5.13967358830592));
#8178=CARTESIAN_POINT('Ctrl Pts',(-0.383362726489432,2.89130175187135,5.15602677059232));
#8179=CARTESIAN_POINT('Ctrl Pts',(-0.326867148839283,2.89544008853964,5.16926500675));
#8180=CARTESIAN_POINT('Ctrl Pts',(-0.269850104507525,2.89957842520793,5.17930868621426));
#8181=CARTESIAN_POINT('Ctrl Pts',(-0.212809518986636,2.90371847051207,5.18935651251147));
#8182=CARTESIAN_POINT('Ctrl Pts',(-0.155247555237378,2.90785851581621,5.19620708965532));
#8183=CARTESIAN_POINT('Ctrl Pts',(-0.0975505429432606,2.91199856112035,
5.19983259638157));
#8184=CARTESIAN_POINT('Ctrl Pts',(-0.0397417314675407,2.91614662856738,
5.20346512823214));
#8185=CARTESIAN_POINT('Ctrl Pts',(0.0182021292546374,2.92029469601441,5.20386009675022));
#8186=CARTESIAN_POINT('Ctrl Pts',(0.0758942242731154,2.92444276346144,5.2010418918398));
#8187=CARTESIAN_POINT('Ctrl Pts',(0.129896919511928,2.92832556269243,5.19840391065973));
#8188=CARTESIAN_POINT('Ctrl Pts',(0.18367870036531,2.93220836192342,5.19295113580138));
#8189=CARTESIAN_POINT('Ctrl Pts',(0.23692976137395,2.93609116115441,5.18474431076452));
#8190=CARTESIAN_POINT('Ctrl Pts',(0.293834898607228,2.94024039722414,5.17597433517856));
#8191=CARTESIAN_POINT('Ctrl Pts',(0.350371063130971,2.94438963329388,5.16402229316462));
#8192=CARTESIAN_POINT('Ctrl Pts',(0.406155507456965,2.94853886936361,5.14893299718094));
#8193=CARTESIAN_POINT('Ctrl Pts',(0.461841333946411,2.95268077025793,5.13387037662162));
#8194=CARTESIAN_POINT('Ctrl Pts',(0.516777579703641,2.95682267115225,5.11568164538636));
#8195=CARTESIAN_POINT('Ctrl Pts',(0.570590348551129,2.96096457204657,5.09446285095979));
#8196=CARTESIAN_POINT('Ctrl Pts',(0.624349914882789,2.9651023780104,5.07326503470012));
#8197=CARTESIAN_POINT('Ctrl Pts',(0.676987723304679,2.96924018397423,5.04904328073132));
#8198=CARTESIAN_POINT('Ctrl Pts',(0.728145436661754,2.97337798993807,5.02194329356025));
#8199=CARTESIAN_POINT('Ctrl Pts',(0.779272206164133,2.97751329306003,4.99485969840536));
#8200=CARTESIAN_POINT('Ctrl Pts',(0.828920196343082,2.98164859618201,4.964901564363));
#8201=CARTESIAN_POINT('Ctrl Pts',(0.876753485845882,2.98578389930398,4.93226161124344));
#8202=CARTESIAN_POINT('Ctrl Pts',(0.924576199211511,2.98991828809341,4.89962887495186));
#8203=CARTESIAN_POINT('Ctrl Pts',(0.970584578814995,2.99405267688284,4.86431579004715));
#8204=CARTESIAN_POINT('Ctrl Pts',(1.01447152341757,2.99818706567227,4.82655848493924));
#8205=CARTESIAN_POINT('Ctrl Pts',(1.05839823980066,3.00232520117965,4.78876696293005));
#8206=CARTESIAN_POINT('Ctrl Pts',(1.10019928310736,3.00646333668704,4.74852713370935));
#8207=CARTESIAN_POINT('Ctrl Pts',(1.13960159336571,3.01060147219443,4.70611466663579));
#8208=CARTESIAN_POINT('Ctrl Pts',(1.17902030680071,3.01474133040709,4.6636845432577));
#8209=CARTESIAN_POINT('Ctrl Pts',(1.21603796238847,3.01888118861976,4.61908037948246));
#8210=CARTESIAN_POINT('Ctrl Pts',(1.25042144777114,3.02302104683242,4.57261144443267));
#8211=CARTESIAN_POINT('Ctrl Pts',(1.28487178165961,3.0271689537735,4.52605216429891));
#8212=CARTESIAN_POINT('Ctrl Pts',(1.31667742338708,3.03131686071457,4.4776213038563));
#8213=CARTESIAN_POINT('Ctrl Pts',(1.34564884130234,3.03546476765565,4.42765688946131));
#8214=CARTESIAN_POINT('Ctrl Pts',(1.37278148105619,3.0393494123456,4.38086365137207));
#8215=CARTESIAN_POINT('Ctrl Pts',(1.3974285397566,3.04323405703554,4.33272591740904));
#8216=CARTESIAN_POINT('Ctrl Pts',(1.41947265623264,3.04711870172549,4.28353724173009));
#8217=CARTESIAN_POINT('Ctrl Pts',(1.4452163205397,3.05165528585027,4.22609348998056));
#8218=CARTESIAN_POINT('Ctrl Pts',(1.46750340567379,3.05619186997506,4.1670086888806));
#8219=CARTESIAN_POINT('Ctrl Pts',(1.48614312745063,3.06072845409985,4.1066970425541));
#8220=CARTESIAN_POINT('Ctrl Pts',(1.50472689290404,3.06525141942863,4.04656645139723));
#8221=CARTESIAN_POINT('Ctrl Pts',(1.5196849767674,3.06977438475741,3.9852166812314));
#8222=CARTESIAN_POINT('Ctrl Pts',(1.53087461175194,3.07429735008618,3.92308119827525));
#8223=CARTESIAN_POINT('Ctrl Pts',(1.54201174785395,3.07879909482771,3.86123723898596));
#8224=CARTESIAN_POINT('Ctrl Pts',(1.54941557119274,3.08330083956923,3.79861525544648));
#8225=CARTESIAN_POINT('Ctrl Pts',(1.55299366908018,3.08780258431076,3.73566062146206));
#8226=CARTESIAN_POINT('Ctrl Pts',(1.55465051858957,3.0898871314084,3.70650927968446));
#8227=CARTESIAN_POINT('Ctrl Pts',(1.55548775667918,3.09197167850605,3.67728683394469));
#8228=CARTESIAN_POINT('Ctrl Pts',(1.55549986667069,3.0940562256037,3.64803850823206));
#8229=CARTESIAN_POINT('',(-0.903606778650208,2.5,2.38126847156104));
#8230=CARTESIAN_POINT('Origin',(-5.55111512312578E-16,2.5,3.64739446828387));
#8231=CARTESIAN_POINT('Ctrl Pts',(-0.903606778650211,2.5,2.38126847156104));
#8232=CARTESIAN_POINT('Ctrl Pts',(-0.951845303079983,2.50424458524762,2.41569526461295));
#8233=CARTESIAN_POINT('Ctrl Pts',(-0.998152286150682,2.50848917049524,2.45290980505554));
#8234=CARTESIAN_POINT('Ctrl Pts',(-1.04220403534506,2.51273375574287,2.49266896033383));
#8235=CARTESIAN_POINT('Ctrl Pts',(-1.0862342553778,2.5169762665584,2.53240868434557));
#8236=CARTESIAN_POINT('Ctrl Pts',(-1.12801106716941,2.52121877737394,2.57469023195131));
#8237=CARTESIAN_POINT('Ctrl Pts',(-1.16724434287758,2.52546128818948,2.61923062238172));
#8238=CARTESIAN_POINT('Ctrl Pts',(-1.20646784811623,2.52970274247018,2.66375992068386));
#8239=CARTESIAN_POINT('Ctrl Pts',(-1.24314875403147,2.53394419675088,2.71054658023795));
#8240=CARTESIAN_POINT('Ctrl Pts',(-1.27703555050147,2.53818565103158,2.75927260009494));
#8241=CARTESIAN_POINT('Ctrl Pts',(-1.3109241886902,2.54242733583174,2.80800126816989));
#8242=CARTESIAN_POINT('Ctrl Pts',(-1.34201813870958,2.54666902063189,2.85866910663535));
#8243=CARTESIAN_POINT('Ctrl Pts',(-1.37010880618711,2.55091070543205,2.91092850898329));
#8244=CARTESIAN_POINT('Ctrl Pts',(-1.39820952338904,2.55515390773844,2.96320660766839));
#8245=CARTESIAN_POINT('Ctrl Pts',(-1.42330459453232,2.55939711004483,3.01707697287849));
#8246=CARTESIAN_POINT('Ctrl Pts',(-1.44523186702567,2.56364031235123,3.07216833837189));
#8247=CARTESIAN_POINT('Ctrl Pts',(-1.46719221439394,2.56788991506085,3.12734280312097));
#8248=CARTESIAN_POINT('Ctrl Pts',(-1.48597504305491,2.57213951777047,3.18374149258924));
#8249=CARTESIAN_POINT('Ctrl Pts',(-1.50146706506275,2.57638912048008,3.24097485442173));
#8250=CARTESIAN_POINT('Ctrl Pts',(-1.51697108246425,2.58064201363542,3.29825253175453));
#8251=CARTESIAN_POINT('Ctrl Pts',(-1.52917911615242,2.58489490679075,3.35636569303991));
#8252=CARTESIAN_POINT('Ctrl Pts',(-1.53802901468286,2.58914779994608,3.41491436162167));
#8253=CARTESIAN_POINT('Ctrl Pts',(-1.5468976907274,2.59340971679371,3.47358725744129));
#8254=CARTESIAN_POINT('Ctrl Pts',(-1.55239394856734,2.59767163364134,3.53269702190671));
#8255=CARTESIAN_POINT('Ctrl Pts',(-1.55450758299866,2.60193355048897,3.59183887090913));
#8256=CARTESIAN_POINT('Ctrl Pts',(-1.55601092615331,2.60496488051634,3.63390408925213));
#8257=CARTESIAN_POINT('Ctrl Pts',(-1.55580413569243,2.60799621054371,3.67598547779196));
#8258=CARTESIAN_POINT('Ctrl Pts',(-1.55389953165917,2.61102754057108,3.71793874877079));
#8259=CARTESIAN_POINT('Ctrl Pts',(-1.55131896143399,2.61513472499091,3.77478172507797));
#8260=CARTESIAN_POINT('Ctrl Pts',(-1.5456085090895,2.61924190941074,3.83162701942664));
#8261=CARTESIAN_POINT('Ctrl Pts',(-1.53676371753943,2.62334909383056,3.88809662127467));
#8262=CARTESIAN_POINT('Ctrl Pts',(-1.52790694169175,2.62746184330188,3.94464273691164));
#8263=CARTESIAN_POINT('Ctrl Pts',(-1.51590728810265,2.6315745927732,4.00081160376278));
#8264=CARTESIAN_POINT('Ctrl Pts',(-1.50081279014695,2.63568734224451,4.05622355106947));
#8265=CARTESIAN_POINT('Ctrl Pts',(-1.48578618297733,2.63978159373098,4.1113862710967));
#8266=CARTESIAN_POINT('Ctrl Pts',(-1.46769260897502,2.64387584521744,4.16579833998209));
#8267=CARTESIAN_POINT('Ctrl Pts',(-1.44663091606904,2.64797009670391,4.21909302755551));
#8268=CARTESIAN_POINT('Ctrl Pts',(-1.42558455612138,2.65206136756637,4.27234891648024));
#8269=CARTESIAN_POINT('Ctrl Pts',(-1.40157455173156,2.65615263842883,4.32448854122648));
#8270=CARTESIAN_POINT('Ctrl Pts',(-1.37474917137091,2.66024390929129,4.3751615778835));
#8271=CARTESIAN_POINT('Ctrl Pts',(-1.34793248907838,2.66433385356855,4.42581818392449));
#8272=CARTESIAN_POINT('Ctrl Pts',(-1.31830248987025,2.66842379784581,4.47500867441785));
#8273=CARTESIAN_POINT('Ctrl Pts',(-1.28605401101194,2.67251374212307,4.52240608578394));
#8274=CARTESIAN_POINT('Ctrl Pts',(-1.25350196148784,2.67664218704132,4.57024967210882));
#8275=CARTESIAN_POINT('Ctrl Pts',(-1.2182821514702,2.68077063195958,4.61626576508545));
#8276=CARTESIAN_POINT('Ctrl Pts',(-1.18063904171929,2.68489907687784,4.66014898106975));
#8277=CARTESIAN_POINT('Ctrl Pts',(-1.14330212489149,2.68899394060087,4.70367524646556));
#8278=CARTESIAN_POINT('Ctrl Pts',(-1.10358160406713,2.6930888043239,4.7451028578062));
#8279=CARTESIAN_POINT('Ctrl Pts',(-1.06175385752749,2.69718366804694,4.78417017000585));
#8280=CARTESIAN_POINT('Ctrl Pts',(-1.01941157894819,2.70132890356281,4.82371805755304));
#8281=CARTESIAN_POINT('Ctrl Pts',(-0.974910298315904,2.70547413907868,4.86084680903068));
#8282=CARTESIAN_POINT('Ctrl Pts',(-0.92856965375026,2.70961937459455,4.89532821978438));
#8283=CARTESIAN_POINT('Ctrl Pts',(-0.882229009184617,2.71376461011042,4.92980963053807));
#8284=CARTESIAN_POINT('Ctrl Pts',(-0.834049506379406,2.71790984562629,4.96164345442314));
#8285=CARTESIAN_POINT('Ctrl Pts',(-0.78437668455737,2.72205508114216,4.99064927163385));
#8286=CARTESIAN_POINT('Ctrl Pts',(-0.734596789904455,2.72620925196883,5.01971761267242));
#8287=CARTESIAN_POINT('Ctrl Pts',(-0.683096214577692,2.7303634227955,5.04607495812685));
#8288=CARTESIAN_POINT('Ctrl Pts',(-0.630201320826871,2.73451759362217,5.06951490805965));
#8289=CARTESIAN_POINT('Ctrl Pts',(-0.57740037556843,2.73866438607905,5.09291322546801));
#8290=CARTESIAN_POINT('Ctrl Pts',(-0.523210498602592,2.74281117853593,5.11340422484301));
#8291=CARTESIAN_POINT('Ctrl Pts',(-0.467983399567077,2.74695797099281,5.1308269027849));
#8292=CARTESIAN_POINT('Ctrl Pts',(-0.412811236673254,2.75110063850411,5.14823224983814));
#8293=CARTESIAN_POINT('Ctrl Pts',(-0.356604388684699,2.75524330601541,5.16257516809759));
#8294=CARTESIAN_POINT('Ctrl Pts',(-0.299733729231309,2.7593859735267,5.1737430331802));
#8295=CARTESIAN_POINT('Ctrl Pts',(-0.242897963352596,2.76352609926199,5.18490404610499));
#8296=CARTESIAN_POINT('Ctrl Pts',(-0.185399701714465,2.76766622499727,5.19289376819827));
#8297=CARTESIAN_POINT('Ctrl Pts',(-0.127622009920969,2.77180635073256,5.19765021253504));
#8298=CARTESIAN_POINT('Ctrl Pts',(-0.0698577464276305,2.77594551424783,
5.20240555141119));
#8299=CARTESIAN_POINT('Ctrl Pts',(-0.0118146987146111,2.78008467776311,
5.20392906193616));
#8300=CARTESIAN_POINT('Ctrl Pts',(0.0461191024158557,2.78422384127839,5.20221062410177));
#8301=CARTESIAN_POINT('Ctrl Pts',(0.104103724821396,2.78836663579255,5.20049067880196));
#8302=CARTESIAN_POINT('Ctrl Pts',(0.161978389084628,2.79250943030672,5.19552311584121));
#8303=CARTESIAN_POINT('Ctrl Pts',(0.219356586646835,2.79665222482088,5.18734996695734));
#8304=CARTESIAN_POINT('Ctrl Pts',(0.276757871024163,2.80079668623877,5.17917352950768));
#8305=CARTESIAN_POINT('Ctrl Pts',(0.3336617800461,2.80494114765666,5.16778903477395));
#8306=CARTESIAN_POINT('Ctrl Pts',(0.389691619463284,2.80908560907455,5.15328978062138));
#8307=CARTESIAN_POINT('Ctrl Pts',(0.445828152477652,2.81323796249251,5.13876291658097));
#8308=CARTESIAN_POINT('Ctrl Pts',(0.501086793044856,2.81739031591048,5.12110959723251));
#8309=CARTESIAN_POINT('Ctrl Pts',(0.555106538707356,2.82154266932844,5.10047291788126));
#8310=CARTESIAN_POINT('Ctrl Pts',(0.605149267896905,2.82538932012337,5.08135554249414));
#8311=CARTESIAN_POINT('Ctrl Pts',(0.65412871360423,2.8292359709183,5.05967858632402));
#8312=CARTESIAN_POINT('Ctrl Pts',(0.701776811900781,2.83308262171323,5.03559098040972));
#8313=CARTESIAN_POINT('Ctrl Pts',(0.753250629317281,2.83723812440404,5.00956935366784));
#8314=CARTESIAN_POINT('Ctrl Pts',(0.803378780995946,2.84139362709485,4.98062856210418));
#8315=CARTESIAN_POINT('Ctrl Pts',(0.85181079741487,2.84554912978566,4.94893148865918));
#8316=CARTESIAN_POINT('Ctrl Pts',(0.900159631423033,2.84969749536434,4.91728885521438));
#8317=CARTESIAN_POINT('Ctrl Pts',(0.946817682329863,2.85384586094302,4.88289961882828));
#8318=CARTESIAN_POINT('Ctrl Pts',(0.991458942442062,2.8579942265217,4.84597254894932));
#8319=CARTESIAN_POINT('Ctrl Pts',(1.03605738133996,2.86213861286568,4.8090809006057));
#8320=CARTESIAN_POINT('Ctrl Pts',(1.07864246529873,2.86628299920966,4.76965657176451));
#8321=CARTESIAN_POINT('Ctrl Pts',(1.11891851883289,2.87042738555364,4.72795062055585));
#8322=CARTESIAN_POINT('Ctrl Pts',(1.15917125850317,2.87456937291235,4.68626881090983));
#8323=CARTESIAN_POINT('Ctrl Pts',(1.19711725811528,2.87871136027106,4.64230836973605));
#8324=CARTESIAN_POINT('Ctrl Pts',(1.23249683959235,2.88285334762977,4.59635800309164));
#8325=CARTESIAN_POINT('Ctrl Pts',(1.26786939829556,2.88699451281254,4.55041675750013));
#8326=CARTESIAN_POINT('Ctrl Pts',(1.30067623431273,2.89113567799531,4.50248678159935));
#8327=CARTESIAN_POINT('Ctrl Pts',(1.33069860539264,2.89527684317808,4.45288901923136));
#8328=CARTESIAN_POINT('Ctrl Pts',(1.36074879240209,2.89942184517836,4.40324530420158));
#8329=CARTESIAN_POINT('Ctrl Pts',(1.38800908947886,2.90356684717864,4.35193115929334));
#8330=CARTESIAN_POINT('Ctrl Pts',(1.4123054265734,2.90771184917893,4.29929448521234));
#8331=CARTESIAN_POINT('Ctrl Pts',(1.43661221496204,2.91185863419015,4.24663516897915));
#8332=CARTESIAN_POINT('Ctrl Pts',(1.45795230958076,2.91600541920138,4.19265267234776));
#8333=CARTESIAN_POINT('Ctrl Pts',(1.47620006451295,2.92015220421261,4.13771438377982));
#8334=CARTESIAN_POINT('Ctrl Pts',(1.49448328890889,2.92430704962585,4.08266930773903));
#8335=CARTESIAN_POINT('Ctrl Pts',(1.50966202478598,2.92846189503909,4.02666522918658));
#8336=CARTESIAN_POINT('Ctrl Pts',(1.52166098851939,2.93261674045233,3.97008330604899));
#8337=CARTESIAN_POINT('Ctrl Pts',(1.53272511068826,2.93644788106299,3.91790969138913));
#8338=CARTESIAN_POINT('Ctrl Pts',(1.54108617161882,2.94027902167365,3.86524520012911));
#8339=CARTESIAN_POINT('Ctrl Pts',(1.54672433177784,2.94411016228431,3.81239171518941));
#8340=CARTESIAN_POINT('Ctrl Pts',(1.55252937411617,2.94805469965497,3.75797383610294));
#8341=CARTESIAN_POINT('Ctrl Pts',(1.5554635597827,2.95199923702563,3.7032412811352));
#8342=CARTESIAN_POINT('Ctrl Pts',(1.55549966270667,2.95594377439629,3.64841883122548));
#8343=CARTESIAN_POINT('Origin',(-2.67773308947627E-16,1.2059437743963,3.64739446828387));
#8344=CARTESIAN_POINT('',(1.55549937976474,3.7940562256037,3.64600538531537));
#8345=CARTESIAN_POINT('',(1.55328922867418,3.65594309057409,3.64812360962188));
#8346=CARTESIAN_POINT('',(1.5555,1.2059437743963,3.64739446828386));
#8347=CARTESIAN_POINT('Ctrl Pts',(1.55320831614475,3.0940562256037,3.64803755943733));
#8348=CARTESIAN_POINT('Ctrl Pts',(1.55211225787393,3.11541956450132,3.34872916974666));
#8349=CARTESIAN_POINT('Ctrl Pts',(1.32451511527677,3.1737920835893,2.5293530162389));
#8350=CARTESIAN_POINT('Ctrl Pts',(-0.00194386449727044,3.26917378286764,
1.80949553386703));
#8351=CARTESIAN_POINT('Ctrl Pts',(-1.54419526187211,3.38020132343872,2.6507072563878));
#8352=CARTESIAN_POINT('Ctrl Pts',(-1.67560476579265,3.4912288640098,4.40256135417452));
#8353=CARTESIAN_POINT('Ctrl Pts',(-0.276097817182277,3.60225640458088,5.46444788548381));
#8354=CARTESIAN_POINT('Ctrl Pts',(1.22562677556159,3.70319885844551,4.92053574953289));
#8355=CARTESIAN_POINT('Ctrl Pts',(1.55162911722742,3.76713213211979,4.02218696309102));
#8356=CARTESIAN_POINT('Ctrl Pts',(1.5548981372976,3.7940562256037,3.64600592223341));
#8357=CARTESIAN_POINT('Ctrl Pts',(1.55731930826876,2.95594474730389,3.64840649193144));
#8358=CARTESIAN_POINT('Ctrl Pts',(1.55406984475527,2.98900906582105,3.18832795677562));
#8359=CARTESIAN_POINT('Ctrl Pts',(1.09493216072152,3.05908256452858,2.20731900520876));
#8360=CARTESIAN_POINT('Ctrl Pts',(-0.571437519320521,3.16616524342647,1.90065774706199));
#8361=CARTESIAN_POINT('Ctrl Pts',(-1.77703909951801,3.27719278399755,3.17828914298809));
#8362=CARTESIAN_POINT('Ctrl Pts',(-1.35908642417454,3.38822032456863,4.88467959896744));
#8363=CARTESIAN_POINT('Ctrl Pts',(0.300609421841398,3.4992478651397,5.4605432395681));
#8364=CARTESIAN_POINT('Ctrl Pts',(1.41386361340157,3.58848878714153,4.59192891748905));
#8365=CARTESIAN_POINT('Ctrl Pts',(1.55417851871196,3.64072052895299,3.86136782353057));
#8366=CARTESIAN_POINT('Ctrl Pts',(1.55328922867418,3.65594309057409,3.64812360962188));
#8367=CARTESIAN_POINT('Origin',(-2.67773308947627E-16,1.2059437743963,3.64739446828387));
#8368=CARTESIAN_POINT('',(1.55549997006787,4.49405622566528,3.64769962209175));
#8369=CARTESIAN_POINT('',(1.5555,4.35539415465377,3.64739446822635));
#8370=CARTESIAN_POINT('',(1.5555,1.2059437743963,3.64739446828386));
#8371=CARTESIAN_POINT('Ctrl Pts',(1.55549937976474,3.7940562256037,3.64600538531537));
#8372=CARTESIAN_POINT('Ctrl Pts',(1.55543459285259,3.79924672256036,3.57345680185905));
#8373=CARTESIAN_POINT('Ctrl Pts',(1.55029041969615,3.80443721951702,3.50113325274295));
#8374=CARTESIAN_POINT('Ctrl Pts',(1.54018379952597,3.80962771647368,3.4296466469911));
#8375=CARTESIAN_POINT('Ctrl Pts',(1.53065335188231,3.81452230622346,3.36223545097616));
#8376=CARTESIAN_POINT('Ctrl Pts',(1.5167106747383,3.81941689597325,3.29556811307819));
#8377=CARTESIAN_POINT('Ctrl Pts',(1.49849211920356,3.82431148572304,3.23013960769527));
#8378=CARTESIAN_POINT('Ctrl Pts',(1.48305092809396,3.82845990987145,3.17468548271226));
#8379=CARTESIAN_POINT('Ctrl Pts',(1.46449498927747,3.83260833401987,3.11997351657152));
#8380=CARTESIAN_POINT('Ctrl Pts',(1.44291390367819,3.83675675816828,3.06637836130218));
#8381=CARTESIAN_POINT('Ctrl Pts',(1.42137112324434,3.84089781910633,3.01287833430057));
#8382=CARTESIAN_POINT('Ctrl Pts',(1.39681404658784,3.84503888004438,2.96049166264535));
#8383=CARTESIAN_POINT('Ctrl Pts',(1.3693821080243,3.84917994098242,2.9095781685026));
#8384=CARTESIAN_POINT('Ctrl Pts',(1.34197740488627,3.85331689052468,2.85871522312709));
#8385=CARTESIAN_POINT('Ctrl Pts',(1.31170374076445,3.85745384006693,2.80932301343158));
#8386=CARTESIAN_POINT('Ctrl Pts',(1.27874802547175,3.86159078960918,2.76174005636458));
#8387=CARTESIAN_POINT('Ctrl Pts',(1.24581236754328,3.86572522133919,2.71418605903015));
#8388=CARTESIAN_POINT('Ctrl Pts',(1.21019819009312,3.86985965306919,2.66843955871361));
#8389=CARTESIAN_POINT('Ctrl Pts',(1.17213644518852,3.87399408479919,2.62481126684703));
#8390=CARTESIAN_POINT('Ctrl Pts',(1.13408324191106,3.87812758870062,2.58119276582432));
#8391=CARTESIAN_POINT('Ctrl Pts',(1.09358390378644,3.88226109260205,2.53969192169267));
#8392=CARTESIAN_POINT('Ctrl Pts',(1.05090908617986,3.88639459650348,2.50058570367461));
#8393=CARTESIAN_POINT('Ctrl Pts',(1.00819573351749,3.89053183292944,2.46144417302074));
#8394=CARTESIAN_POINT('Ctrl Pts',(0.963303359719073,3.8946690693554,2.42470194310747));
#8395=CARTESIAN_POINT('Ctrl Pts',(0.916537863760172,3.89880630578136,2.39059751002293));
#8396=CARTESIAN_POINT('Ctrl Pts',(0.869752999509781,3.90294525567575,2.35647895232393));
#8397=CARTESIAN_POINT('Ctrl Pts',(0.821093903997002,3.90708420557015,2.32500065384963));
#8398=CARTESIAN_POINT('Ctrl Pts',(0.770895120881294,3.91122315546454,2.29635747300898));
#8399=CARTESIAN_POINT('Ctrl Pts',(0.720598766603014,3.91537015021835,2.26765861853878));
#8400=CARTESIAN_POINT('Ctrl Pts',(0.668757211424777,3.91951714497215,2.24180612807529));
#8401=CARTESIAN_POINT('Ctrl Pts',(0.615728403904911,3.92366413972596,2.21894818556103));
#8402=CARTESIAN_POINT('Ctrl Pts',(0.565965033127361,3.92755576858201,2.19749780185924));
#8403=CARTESIAN_POINT('Ctrl Pts',(0.515156658330857,3.93144739743807,2.17868417709866));
#8404=CARTESIAN_POINT('Ctrl Pts',(0.46361041530187,3.93533902629412,2.16258955422155));
#8405=CARTESIAN_POINT('Ctrl Pts',(0.408662882562632,3.93948744510044,2.14543292426175));
#8406=CARTESIAN_POINT('Ctrl Pts',(0.352646623653704,3.94363586390677,2.13129460873933));
#8407=CARTESIAN_POINT('Ctrl Pts',(0.29592487144026,3.94778428271309,2.12030287952337));
#8408=CARTESIAN_POINT('Ctrl Pts',(0.239303797818613,3.95192533826022,2.10933066013875));
#8409=CARTESIAN_POINT('Ctrl Pts',(0.181980223358933,3.95606639380735,2.10149403971228));
#8410=CARTESIAN_POINT('Ctrl Pts',(0.12433199791367,3.96020744935448,2.0968713938684));
#8411=CARTESIAN_POINT('Ctrl Pts',(0.0667410081572819,3.96434439347988,2.09225333759024));
#8412=CARTESIAN_POINT('Ctrl Pts',(0.00882652245797441,3.96848133760527,
2.09084297499291));
#8413=CARTESIAN_POINT('Ctrl Pts',(-0.0490257099392019,3.97261828173067,
2.09266724791209));
#8414=CARTESIAN_POINT('Ctrl Pts',(-0.10684273228549,3.97675270802733,2.09449041054149));
#8415=CARTESIAN_POINT('Ctrl Pts',(-0.164597057061184,3.98088713432399,2.09954428982219));
#8416=CARTESIAN_POINT('Ctrl Pts',(-0.221902358276799,3.98502156062065,2.10780374559449));
#8417=CARTESIAN_POINT('Ctrl Pts',(-0.279194799207534,3.98915505908169,2.11606134780436));
#8418=CARTESIAN_POINT('Ctrl Pts',(-0.336037901517815,3.99328855754272,2.12752302405911));
#8419=CARTESIAN_POINT('Ctrl Pts',(-0.392052103871645,3.99742205600376,2.14211197059454));
#8420=CARTESIAN_POINT('Ctrl Pts',(-0.44811688716568,4.00155928702242,2.15671409097877));
#8421=CARTESIAN_POINT('Ctrl Pts',(-0.503350769331993,4.00569651804109,2.17444899447387));
#8422=CARTESIAN_POINT('Ctrl Pts',(-0.557387348271533,4.00983374905976,2.19518938841848));
#8423=CARTESIAN_POINT('Ctrl Pts',(-0.611446307026563,4.01397269355601,2.21593837221462));
#8424=CARTESIAN_POINT('Ctrl Pts',(-0.664306497514911,4.01811163805226,2.23969511520848));
#8425=CARTESIAN_POINT('Ctrl Pts',(-0.715622597532242,4.02225058254852,2.26628457117169));
#8426=CARTESIAN_POINT('Ctrl Pts',(-0.767038441642636,4.02639757199099,2.29292570957315));
#8427=CARTESIAN_POINT('Ctrl Pts',(-0.816903747256544,4.03054456143347,2.32241029888276));
#8428=CARTESIAN_POINT('Ctrl Pts',(-0.864899667938166,4.03469155087595,2.35451828921626));
#8429=CARTESIAN_POINT('Ctrl Pts',(-0.909940626698667,4.03858322287236,2.38464948886732));
#8430=CARTESIAN_POINT('Ctrl Pts',(-0.953335299435889,4.04247489486877,2.41709037054295));
#8431=CARTESIAN_POINT('Ctrl Pts',(-0.994847796632108,4.04636656686519,2.4516277219925));
#8432=CARTESIAN_POINT('Ctrl Pts',(-1.03909898735835,4.0505149831588,2.48844359743718));
#8433=CARTESIAN_POINT('Ctrl Pts',(-1.08139645579429,4.05466339945241,2.5277962696892));
#8434=CARTESIAN_POINT('Ctrl Pts',(-1.12143520301905,4.05881181574602,2.56945043660615));
#8435=CARTESIAN_POINT('Ctrl Pts',(-1.16140288229428,4.06295286868638,2.61103066823696));
#8436=CARTESIAN_POINT('Ctrl Pts',(-1.19911944019534,4.06709392162673,2.65490391383242));
#8437=CARTESIAN_POINT('Ctrl Pts',(-1.23431383195748,4.07123497456708,2.70079549604777));
#8438=CARTESIAN_POINT('Ctrl Pts',(-1.26947328068964,4.0753719160303,2.74664151444306));
#8439=CARTESIAN_POINT('Ctrl Pts',(-1.30211520951443,4.07950885749352,2.79450148797204));
#8440=CARTESIAN_POINT('Ctrl Pts',(-1.33200746762014,4.08364579895674,2.84406616914074));
#8441=CARTESIAN_POINT('Ctrl Pts',(-1.36188153230805,4.08778022254043,2.89360068360376));
#8442=CARTESIAN_POINT('Ctrl Pts',(-1.38900897537655,4.09191464612413,2.94483740401328));
#8443=CARTESIAN_POINT('Ctrl Pts',(-1.41320106171709,4.09604906970783,2.99743830886872));
#8444=CARTESIAN_POINT('Ctrl Pts',(-1.43738771866766,4.10018256540968,3.05002740858999));
#8445=CARTESIAN_POINT('Ctrl Pts',(-1.45864010930288,4.10431606111152,3.103979612102));
#8446=CARTESIAN_POINT('Ctrl Pts',(-1.47681655061521,4.10844955681337,3.15893451513622));
#8447=CARTESIAN_POINT('Ctrl Pts',(-1.49500940507868,4.11258678502195,3.2139390419177));
#8448=CARTESIAN_POINT('Ctrl Pts',(-1.51012059463379,4.11672401323054,3.26994758241586));
#8449=CARTESIAN_POINT('Ctrl Pts',(-1.52205797546509,4.12086124143913,3.32658335668842));
#8450=CARTESIAN_POINT('Ctrl Pts',(-1.53400030019751,4.12500018309285,3.3832425868322));
#8451=CARTESIAN_POINT('Ctrl Pts',(-1.5427661155984,4.12913912474657,3.44052905299625));
#8452=CARTESIAN_POINT('Ctrl Pts',(-1.54831482273191,4.1332780664003,3.49805773566704));
#8453=CARTESIAN_POINT('Ctrl Pts',(-1.55387431497743,4.13742505298202,3.55569823777111));
#8454=CARTESIAN_POINT('Ctrl Pts',(-1.55620418080109,4.14157203956375,3.61358137509542));
#8455=CARTESIAN_POINT('Ctrl Pts',(-1.55531598818641,4.14571902614547,3.67131991272537));
#8456=CARTESIAN_POINT('Ctrl Pts',(-1.55448247363523,4.14961071990907,3.72550400577358));
#8457=CARTESIAN_POINT('Ctrl Pts',(-1.55081545093387,4.15350241367267,3.77956041061299));
#8458=CARTESIAN_POINT('Ctrl Pts',(-1.5443658084111,4.15739410743627,3.83317525257204));
#8459=CARTESIAN_POINT('Ctrl Pts',(-1.53749069896047,4.16154252658953,3.89032693273814));
#8460=CARTESIAN_POINT('Ctrl Pts',(-1.52742442723014,4.16569094574279,3.94721615662609));
#8461=CARTESIAN_POINT('Ctrl Pts',(-1.51419888969869,4.16983936489604,4.00345903045659));
#8462=CARTESIAN_POINT('Ctrl Pts',(-1.50099682699795,4.17398042076163,4.05960207530557));
#8463=CARTESIAN_POINT('Ctrl Pts',(-1.48464674700967,4.17812147662723,4.115100544536));
#8464=CARTESIAN_POINT('Ctrl Pts',(-1.46523204945129,4.18226253249282,4.16957766531415));
#8465=CARTESIAN_POINT('Ctrl Pts',(-1.44583662773766,4.18639947691915,4.22400069858879));
#8466=CARTESIAN_POINT('Ctrl Pts',(-1.42338279090196,4.19053642134547,4.27740390454189));
#8467=CARTESIAN_POINT('Ctrl Pts',(-1.39800409065944,4.19467336577179,4.32942438881484));
#8468=CARTESIAN_POINT('Ctrl Pts',(-1.37264083652224,4.19880779235131,4.38141321213309));
#8469=CARTESIAN_POINT('Ctrl Pts',(-1.34435647560062,4.20294221893083,4.43202051497412));
#8470=CARTESIAN_POINT('Ctrl Pts',(-1.31333230115958,4.20707664551035,4.48090422631367));
#8471=CARTESIAN_POINT('Ctrl Pts',(-1.28231508921055,4.21121014423562,4.529776967097));
#8472=CARTESIAN_POINT('Ctrl Pts',(-1.24855956333046,4.21534364296089,4.57692644490255));
#8473=CARTESIAN_POINT('Ctrl Pts',(-1.21229136733349,4.21947714168616,4.62203793678336));
#8474=CARTESIAN_POINT('Ctrl Pts',(-1.1759904213609,4.22361437293737,4.66719016408588));
#8475=CARTESIAN_POINT('Ctrl Pts',(-1.13717259725465,4.22775160418858,4.71030032036805));
#8476=CARTESIAN_POINT('Ctrl Pts',(-1.09610419663964,4.2318888354398,4.75108638186709));
#8477=CARTESIAN_POINT('Ctrl Pts',(-1.0550187872851,4.23602778015166,4.7918893351731));
#8478=CARTESIAN_POINT('Ctrl Pts',(-1.01168133261275,4.24016672486353,4.83036592741652));
#8479=CARTESIAN_POINT('Ctrl Pts',(-0.96639305027996,4.2443056695754,4.86627293735722));
#8480=CARTESIAN_POINT('Ctrl Pts',(-0.921016740592843,4.24845265920163,4.9022497401654));
#8481=CARTESIAN_POINT('Ctrl Pts',(-0.873682452134067,4.25259964882785,4.93564667763783));
#8482=CARTESIAN_POINT('Ctrl Pts',(-0.824721598466733,4.25674663845408,4.96626312551342));
#8483=CARTESIAN_POINT('Ctrl Pts',(-0.778775142055082,4.26063830830517,4.99499459529852));
#8484=CARTESIAN_POINT('Ctrl Pts',(-0.731396819639847,4.26452997815626,5.02127767127383));
#8485=CARTESIAN_POINT('Ctrl Pts',(-0.682877801894672,4.26842164800735,5.04498459334898));
#8486=CARTESIAN_POINT('Ctrl Pts',(-0.631157796762294,4.27257006638072,5.07025555282798));
#8487=CARTESIAN_POINT('Ctrl Pts',(-0.577924791530158,4.27671848475409,5.09270459408808));
#8488=CARTESIAN_POINT('Ctrl Pts',(-0.523518435833301,4.28086690312746,5.11214997598564));
#8489=CARTESIAN_POINT('Ctrl Pts',(-0.469208649529518,4.2850079582022,5.13156084300522));
#8490=CARTESIAN_POINT('Ctrl Pts',(-0.413730132841114,4.28914901327694,5.14797845897071));
#8491=CARTESIAN_POINT('Ctrl Pts',(-0.357444531875422,4.29329006835168,5.16126819374196));
#8492=CARTESIAN_POINT('Ctrl Pts',(-0.301214814053124,4.29742701198103,5.17454473380371));
#8493=CARTESIAN_POINT('Ctrl Pts',(-0.24418010380913,4.30156395561038,5.18469942661238));
#8494=CARTESIAN_POINT('Ctrl Pts',(-0.186717636011615,4.30570089923973,5.19164728903643));
#8495=CARTESIAN_POINT('Ctrl Pts',(-0.129290141367093,4.30983532501754,5.19859092281064));
#8496=CARTESIAN_POINT('Ctrl Pts',(-0.0714359211261828,4.31396975079536,
5.20233153280199));
#8497=CARTESIAN_POINT('Ctrl Pts',(-0.013540658583629,4.31810417657318,5.20283553131555));
#8498=CARTESIAN_POINT('Ctrl Pts',(0.044341610967578,4.32223767449342,5.20333941672058));
#8499=CARTESIAN_POINT('Ctrl Pts',(0.102264384113867,4.32637117241365,5.20060812818138));
#8500=CARTESIAN_POINT('Ctrl Pts',(0.159840849344005,4.33050467033389,5.19466017037934));
#8501=CARTESIAN_POINT('Ctrl Pts',(0.21746930582411,4.33464190078135,5.1887068416022));
#8502=CARTESIAN_POINT('Ctrl Pts',(0.274750310160414,4.3387791312288,5.17953109150457));
#8503=CARTESIAN_POINT('Ctrl Pts',(0.331302421324793,4.34291636167625,5.167203323247));
#8504=CARTESIAN_POINT('Ctrl Pts',(0.387877953901925,4.34705530558374,5.15487044936662));
#8505=CARTESIAN_POINT('Ctrl Pts',(0.443723488319045,4.35119424949122,5.13938309309894));
#8506=CARTESIAN_POINT('Ctrl Pts',(0.498471197309759,4.3553331933987,5.12086205036791));
#8507=CARTESIAN_POINT('Ctrl Pts',(0.553325320197712,4.35948018223007,5.10230500802385));
#8508=CARTESIAN_POINT('Ctrl Pts',(0.607076868142722,4.36362717106143,5.0807026894981));
#8509=CARTESIAN_POINT('Ctrl Pts',(0.659377377398335,4.3677741598928,5.05622438142999));
#8510=CARTESIAN_POINT('Ctrl Pts',(0.708457964997536,4.37166583612134,5.0332530994957));
#8511=CARTESIAN_POINT('Ctrl Pts',(0.756260586977096,4.37555751234989,5.00774967826566));
#8512=CARTESIAN_POINT('Ctrl Pts',(0.80251981524134,4.37944918857843,4.97988919478188));
#8513=CARTESIAN_POINT('Ctrl Pts',(0.851830855280501,4.38359760630016,4.95019070070559));
#8514=CARTESIAN_POINT('Ctrl Pts',(0.899594386513453,4.3877460240219,4.91768906526787));
#8515=CARTESIAN_POINT('Ctrl Pts',(0.945473326109702,4.39189444174363,4.88257074704535));
#8516=CARTESIAN_POINT('Ctrl Pts',(0.99127083205346,4.39603549615641,4.84751476271606));
#8517=CARTESIAN_POINT('Ctrl Pts',(1.03518997586039,4.40017655056918,4.80985162826572));
#8518=CARTESIAN_POINT('Ctrl Pts',(1.07692128200614,4.40431760498195,4.76981186050578));
#8519=CARTESIAN_POINT('Ctrl Pts',(1.11861115517062,4.40845454794349,4.72981184628105));
#8520=CARTESIAN_POINT('Ctrl Pts',(1.15811712064237,4.41259149090503,4.68744023260774));
#8521=CARTESIAN_POINT('Ctrl Pts',(1.19516291999959,4.41672843386657,4.64296759199607));
#8522=CARTESIAN_POINT('Ctrl Pts',(1.23218617227358,4.42086285897187,4.59852201864564));
#8523=CARTESIAN_POINT('Ctrl Pts',(1.26675189399722,4.42499728407717,4.55197835246778));
#8524=CARTESIAN_POINT('Ctrl Pts',(1.29862239032697,4.42913170918246,4.50364217621742));
#8525=CARTESIAN_POINT('Ctrl Pts',(1.33048573417583,4.43326520642657,4.45531684772963));
#8526=CARTESIAN_POINT('Ctrl Pts',(1.35965476700255,4.43739870367068,4.40520024231475));
#8527=CARTESIAN_POINT('Ctrl Pts',(1.38593491887229,4.44153220091479,4.35362718534706));
#8528=CARTESIAN_POINT('Ctrl Pts',(1.41223880158493,4.4456694306858,4.30200755817238));
#8529=CARTESIAN_POINT('Ctrl Pts',(1.4356483522893,4.4498066604568,4.248929315779));
#8530=CARTESIAN_POINT('Ctrl Pts',(1.4560154931007,4.45394389022781,4.19475096440931));
#8531=CARTESIAN_POINT('Ctrl Pts',(1.47639106908664,4.45808283345754,4.14055017474775));
#8532=CARTESIAN_POINT('Ctrl Pts',(1.49372156596716,4.46222177668727,4.08524886536955));
#8533=CARTESIAN_POINT('Ctrl Pts',(1.50790861123547,4.46636071991701,4.02922148430278));
#8534=CARTESIAN_POINT('Ctrl Pts',(1.52212323209167,4.47050770807722,3.97308520191503));
#8535=CARTESIAN_POINT('Ctrl Pts',(1.53318209055855,4.47465469623742,3.91622054035924));
#8536=CARTESIAN_POINT('Ctrl Pts',(1.54103804564486,4.47880168439763,3.85901202869666));
#8537=CARTESIAN_POINT('Ctrl Pts',(1.54841035406551,4.48269336598159,3.80532552112007));
#8538=CARTESIAN_POINT('Ctrl Pts',(1.55296246258241,4.48658504756555,3.75133661842237));
#8539=CARTESIAN_POINT('Ctrl Pts',(1.55469719497037,4.49047672914951,3.6973632780683));
#8540=CARTESIAN_POINT('Ctrl Pts',(1.55522905318279,4.49166989463424,3.68081538600244));
#8541=CARTESIAN_POINT('Ctrl Pts',(1.55549672149285,4.49286306011897,3.66425895728588));
#8542=CARTESIAN_POINT('Ctrl Pts',(1.5554999700677,4.4940562256037,3.64769962294641));
#8543=CARTESIAN_POINT('Ctrl Pts',(1.55549987088463,3.65467159675291,3.64802824892935));
#8544=CARTESIAN_POINT('Ctrl Pts',(1.55550680899066,3.6558397976945,3.63099992358026));
#8545=CARTESIAN_POINT('Ctrl Pts',(1.55523412898573,3.65701542995216,3.61397308773208));
#8546=CARTESIAN_POINT('Ctrl Pts',(1.55413408026995,3.65937408981715,3.58006687167519));
#8547=CARTESIAN_POINT('Ctrl Pts',(1.55331107084226,3.66055682043176,3.56318981869217));
#8548=CARTESIAN_POINT('Ctrl Pts',(1.55069027106267,3.66340087943599,3.52293785225933));
#8549=CARTESIAN_POINT('Ctrl Pts',(1.5486386943779,3.66506974526968,3.49958428363513));
#8550=CARTESIAN_POINT('Ctrl Pts',(1.54262409405456,3.66900197693008,3.44523866763588));
#8551=CARTESIAN_POINT('Ctrl Pts',(1.53825361546319,3.67127758602551,3.41430303623448));
#8552=CARTESIAN_POINT('Ctrl Pts',(1.51028537399236,3.68343974554108,3.25182285702067));
#8553=CARTESIAN_POINT('Ctrl Pts',(1.47074125747952,3.69383819776969,3.12361475845923));
#8554=CARTESIAN_POINT('Ctrl Pts',(1.39151303190329,3.70859912506545,2.94985225609737));
#8555=CARTESIAN_POINT('Ctrl Pts',(1.36483055976558,3.71299964536092,2.89898780474795));
#8556=CARTESIAN_POINT('Ctrl Pts',(1.32549190967572,3.71871027510865,2.83313138202807));
#8557=CARTESIAN_POINT('Ctrl Pts',(1.31528024997209,3.72013282285924,2.81673741705178));
#8558=CARTESIAN_POINT('Ctrl Pts',(1.2966262245711,3.7226228050478,2.78799690110064));
#8559=CARTESIAN_POINT('Ctrl Pts',(1.28830732785269,3.72369706600524,2.77557567591207));
#8560=CARTESIAN_POINT('Ctrl Pts',(1.26719687946834,3.72633755331549,2.74501720118994));
#8561=CARTESIAN_POINT('Ctrl Pts',(1.25419411705297,3.72789032617511,2.72703045520652));
#8562=CARTESIAN_POINT('Ctrl Pts',(1.19592062594428,3.73456811992015,2.64995036594936));
#8563=CARTESIAN_POINT('Ctrl Pts',(1.14682172558588,3.73949171494677,2.59386547306114));
#8564=CARTESIAN_POINT('Ctrl Pts',(1.0425410697477,3.7491572560565,2.49071611753265));
#8565=CARTESIAN_POINT('Ctrl Pts',(0.987719652740954,3.75388941824133,2.44356475363856));
#8566=CARTESIAN_POINT('Ctrl Pts',(0.901121842986846,3.76113182859896,2.37899336284216));
#8567=CARTESIAN_POINT('Ctrl Pts',(0.871692903772833,3.76355595621517,2.35859147991404));
#8568=CARTESIAN_POINT('Ctrl Pts',(0.814750259645494,3.76820638574019,2.32195845638407));
#8569=CARTESIAN_POINT('Ctrl Pts',(0.787389467575394,3.77042440273263,2.30552406392175));
#8570=CARTESIAN_POINT('Ctrl Pts',(0.736979070458522,3.77449557003692,2.27731757093331));
#8571=CARTESIAN_POINT('Ctrl Pts',(0.714103896334424,3.77633744759335,2.26525687274253));
#8572=CARTESIAN_POINT('Ctrl Pts',(0.662031327540791,3.78052407799057,2.23943995787138));
#8573=CARTESIAN_POINT('Ctrl Pts',(0.632685878936297,3.78287931487906,2.22601145424455));
#8574=CARTESIAN_POINT('Ctrl Pts',(0.485608225534339,3.79467579654246,2.16416571683604));
#8575=CARTESIAN_POINT('Ctrl Pts',(0.362675252472724,3.80456766130157,2.12942285856927));
#8576=CARTESIAN_POINT('Ctrl Pts',(0.177330195496293,3.81907447215376,2.10085992851241));
#8577=CARTESIAN_POINT('Ctrl Pts',(0.117254235714492,3.82370504365851,2.09514835401264));
#8578=CARTESIAN_POINT('Ctrl Pts',(0.037506588442317,3.82964856040533,2.09222446656055));
#8579=CARTESIAN_POINT('Ctrl Pts',(0.0180072309046056,3.83108561643035,2.09187644622304));
#8580=CARTESIAN_POINT('Ctrl Pts',(-0.0164270910425457,3.8335889385491,2.09190953556467));
#8581=CARTESIAN_POINT('Ctrl Pts',(-0.0313576239195812,3.83466241648109,
2.09213887509024));
#8582=CARTESIAN_POINT('Ctrl Pts',(-0.0682069141322419,3.83728434998413,
2.0932358269107));
#8583=CARTESIAN_POINT('Ctrl Pts',(-0.0901145359935279,3.83881988654501,
2.09435204504922));
#8584=CARTESIAN_POINT('Ctrl Pts',(-0.215852175537578,3.84753727450119,2.10342844313732));
#8585=CARTESIAN_POINT('Ctrl Pts',(-0.318709908064491,3.85430539505901,2.12133652219782));
#8586=CARTESIAN_POINT('Ctrl Pts',(-0.490423267156545,3.86606195438738,2.16936768880608));
#8587=CARTESIAN_POINT('Ctrl Pts',(-0.560303712190142,3.87098351014319,2.19441950024454));
#8588=CARTESIAN_POINT('Ctrl Pts',(-0.658944774022162,3.87836259443022,2.23795954717942));
#8589=CARTESIAN_POINT('Ctrl Pts',(-0.689310208044195,3.88069634274766,2.25255893699465));
#8590=CARTESIAN_POINT('Ctrl Pts',(-0.74214737817428,3.88488549146296,2.28010932246865));
#8591=CARTESIAN_POINT('Ctrl Pts',(-0.764814597393762,3.88672620365825,2.29265837394572));
#8592=CARTESIAN_POINT('Ctrl Pts',(-0.813669412320802,3.89079627301213,2.32132236129594));
#8593=CARTESIAN_POINT('Ctrl Pts',(-0.839713288787418,3.89303318337717,2.33765919423326));
#8594=CARTESIAN_POINT('Ctrl Pts',(-0.975481178202155,3.90507091660595,2.42853824264552));
#8595=CARTESIAN_POINT('Ctrl Pts',(-1.07579959823294,3.91537836815593,2.51610516441592));
#8596=CARTESIAN_POINT('Ctrl Pts',(-1.20329253551976,3.93023958039282,2.6598648928988));
#8597=CARTESIAN_POINT('Ctrl Pts',(-1.24022315403323,3.93481226237697,2.70666307428755));
#8598=CARTESIAN_POINT('Ctrl Pts',(-1.28553665769892,3.94069738495624,2.77140690163983));
#8599=CARTESIAN_POINT('Ctrl Pts',(-1.29639246572693,3.94213095783939,2.78755414106259));
#8600=CARTESIAN_POINT('Ctrl Pts',(-1.31504202698694,3.94463099181762,2.81645055925579));
#8601=CARTESIAN_POINT('Ctrl Pts',(-1.32295931239141,3.94570457421527,2.82911456180254));
#8602=CARTESIAN_POINT('Ctrl Pts',(-1.34208104326949,3.94833055590119,2.86070376855965));
#8603=CARTESIAN_POINT('Ctrl Pts',(-1.35306867879817,3.94986991580466,2.87975583757072));
#8604=CARTESIAN_POINT('Ctrl Pts',(-1.40379912232057,3.95716047724157,2.97219618430925));
#8605=CARTESIAN_POINT('Ctrl Pts',(-1.43800116895929,3.96265200893646,3.04847820183888));
#8606=CARTESIAN_POINT('Ctrl Pts',(-1.48831473982958,3.97255653176303,3.19024780674943));
#8607=CARTESIAN_POINT('Ctrl Pts',(-1.50661116414808,3.97695707524957,3.25472924498367));
#8608=CARTESIAN_POINT('Ctrl Pts',(-1.53066914784216,3.98463974755485,3.36653822113338));
#8609=CARTESIAN_POINT('Ctrl Pts',(-1.53851744739748,3.98786841186561,3.41331832020172));
#8610=CARTESIAN_POINT('Ctrl Pts',(-1.54754519080994,3.99308676380265,3.48786243751191));
#8611=CARTESIAN_POINT('Ctrl Pts',(-1.55013900021884,3.9950318376677,3.51542669523067));
#8612=CARTESIAN_POINT('Ctrl Pts',(-1.5537959718898,3.99890865359388,3.5698165285004));
#8613=CARTESIAN_POINT('Ctrl Pts',(-1.55490289421904,4.0008383074917,3.59662950069242));
#8614=CARTESIAN_POINT('Ctrl Pts',(-1.55595583761273,4.0058148796882,3.66504128398195));
#8615=CARTESIAN_POINT('Ctrl Pts',(-1.55492777078369,4.00889081730036,3.70663136778312));
#8616=CARTESIAN_POINT('Ctrl Pts',(-1.5451581658646,4.02021507583114,3.85717591500449));
#8617=CARTESIAN_POINT('Ctrl Pts',(-1.52661002056277,4.02872846159367,3.96516491297883));
#8618=CARTESIAN_POINT('Ctrl Pts',(-1.48123288127581,4.0416298553189,4.12578027454459));
#8619=CARTESIAN_POINT('Ctrl Pts',(-1.46248512658164,4.04605113103239,4.18035078001403));
#8620=CARTESIAN_POINT('Ctrl Pts',(-1.43346189450557,4.05178295040139,4.25166337019466));
#8621=CARTESIAN_POINT('Ctrl Pts',(-1.42584152590385,4.05320695329046,4.269431403307));
#8622=CARTESIAN_POINT('Ctrl Pts',(-1.41174427596951,4.05569830103502,4.30067986094912));
#8623=CARTESIAN_POINT('Ctrl Pts',(-1.40540142053742,4.05677251003103,4.31421572277038));
#8624=CARTESIAN_POINT('Ctrl Pts',(-1.38916956655271,4.05941129017011,4.34759409175537));
#8625=CARTESIAN_POINT('Ctrl Pts',(-1.37904990282173,4.06096245831637,4.3673202275207));
#8626=CARTESIAN_POINT('Ctrl Pts',(-1.33258346637689,4.06771803553351,4.45331867323996));
#8627=CARTESIAN_POINT('Ctrl Pts',(-1.29185274846998,4.07271401779846,4.51711374837089));
#8628=CARTESIAN_POINT('Ctrl Pts',(-1.20385374876466,4.0824082992758,4.63503528730362));
#8629=CARTESIAN_POINT('Ctrl Pts',(-1.15716490630667,4.0870973463686,4.68934792617555));
#8630=CARTESIAN_POINT('Ctrl Pts',(-1.08186035945384,4.0942852276056,4.76562036350572));
#8631=CARTESIAN_POINT('Ctrl Pts',(-1.05595219040463,4.09669956078723,4.7901173942015));
#8632=CARTESIAN_POINT('Ctrl Pts',(-1.00536851711708,4.10133405586616,4.83475578174981));
#8633=CARTESIAN_POINT('Ctrl Pts',(-0.980871428792829,4.10354607254253,4.85507146753244));
#8634=CARTESIAN_POINT('Ctrl Pts',(-0.935369985281544,4.10761129536025,4.89050822931024));
#8635=CARTESIAN_POINT('Ctrl Pts',(-0.914578126148144,4.1094534041472,4.90588385487769));
#8636=CARTESIAN_POINT('Ctrl Pts',(-0.866924244355616,4.11364728350535,4.93931928796561));
#8637=CARTESIAN_POINT('Ctrl Pts',(-0.839863119069813,4.11600971701675,4.95707268674787));
#8638=CARTESIAN_POINT('Ctrl Pts',(-0.704269964341053,4.12776720776442,5.04009727419382));
#8639=CARTESIAN_POINT('Ctrl Pts',(-0.588614722709753,4.13760696901563,5.0927796949871));
#8640=CARTESIAN_POINT('Ctrl Pts',(-0.410052301755297,4.15209204024159,5.14909841878631));
#8641=CARTESIAN_POINT('Ctrl Pts',(-0.351195803165076,4.15675058905869,5.16394339408206));
#8642=CARTESIAN_POINT('Ctrl Pts',(-0.272443798948656,4.16272218540384,5.17897392928248));
#8643=CARTESIAN_POINT('Ctrl Pts',(-0.253201732900101,4.16416081350884,5.1822723952049));
#8644=CARTESIAN_POINT('Ctrl Pts',(-0.219141589904982,4.16666552363155,5.1874529435621));
#8645=CARTESIAN_POINT('Ctrl Pts',(-0.20435098522404,4.16773886117158,5.189485209551));
#8646=CARTESIAN_POINT('Ctrl Pts',(-0.167793747187085,4.17035850698453,5.19397300024505));
#8647=CARTESIAN_POINT('Ctrl Pts',(-0.146000645682202,4.17189195897003,5.19618232992627));
#8648=CARTESIAN_POINT('Ctrl Pts',(-0.0201587373251121,4.18062243716555,
5.20625972862682));
#8649=CARTESIAN_POINT('Ctrl Pts',(0.084436912459217,4.18740359634424,5.20410360241846));
#8650=CARTESIAN_POINT('Ctrl Pts',(0.261661543953308,4.19917557832372,5.18252119934605));
#8651=CARTESIAN_POINT('Ctrl Pts',(0.334540989733795,4.20409875308634,5.16830259511418));
#8652=CARTESIAN_POINT('Ctrl Pts',(0.438580618066137,4.21147563304065,5.14016296928541));
#8653=CARTESIAN_POINT('Ctrl Pts',(0.470741964500938,4.21380525218522,5.13033494943017));
#8654=CARTESIAN_POINT('Ctrl Pts',(0.527071454822894,4.21799003989888,5.1111044438017));
#8655=CARTESIAN_POINT('Ctrl Pts',(0.55137089440572,4.21983064183916,5.10212509645768));
#8656=CARTESIAN_POINT('Ctrl Pts',(0.604033807235616,4.22390400242875,5.08115563162026));
#8657=CARTESIAN_POINT('Ctrl Pts',(0.632287646929645,4.22614440236699,5.06892181386107));
#8658=CARTESIAN_POINT('Ctrl Pts',(0.77945934922997,4.23812145992238,4.99994128604665));
#8659=CARTESIAN_POINT('Ctrl Pts',(0.891152971316397,4.24835666459975,4.9291013957991));
#8660=CARTESIAN_POINT('Ctrl Pts',(1.0389128326723,4.26320164283447,4.8066462636505));
#8661=CARTESIAN_POINT('Ctrl Pts',(1.08300182460194,4.26782534952738,4.76556847845488));
#8662=CARTESIAN_POINT('Ctrl Pts',(1.13806943313459,4.27376189484348,4.70794065377763));
#8663=CARTESIAN_POINT('Ctrl Pts',(1.15127156698475,4.27519850063877,4.69359431729372));
#8664=CARTESIAN_POINT('Ctrl Pts',(1.17410413686256,4.27770133638679,4.66782706550215));
#8665=CARTESIAN_POINT('Ctrl Pts',(1.18384496852464,4.27877476820537,4.6565100888032));
#8666=CARTESIAN_POINT('Ctrl Pts',(1.20518276318679,4.28114087800315,4.63098531790373));
#8667=CARTESIAN_POINT('Ctrl Pts',(1.21669392899843,4.28242797244065,4.6167099041841));
#8668=CARTESIAN_POINT('Ctrl Pts',(1.29072584311944,4.29080267171439,4.52150271466707));
#8669=CARTESIAN_POINT('Ctrl Pts',(1.345395616747,4.29746748967359,4.43476660068687));
#8670=CARTESIAN_POINT('Ctrl Pts',(1.42707242919979,4.30949517736764,4.27148493600972));
#8671=CARTESIAN_POINT('Ctrl Pts',(1.45737082104823,4.31481006451829,4.19702433963266));
#8672=CARTESIAN_POINT('Ctrl Pts',(1.49195467811449,4.32259461685936,4.08872067062043));
#8673=CARTESIAN_POINT('Ctrl Pts',(1.50109295279395,4.32491140714319,4.05656098880325));
#8674=CARTESIAN_POINT('Ctrl Pts',(1.51545879030476,4.32908270041734,3.9990125973105));
#8675=CARTESIAN_POINT('Ctrl Pts',(1.52110124708772,4.33092301439652,3.97374014819926));
#8676=CARTESIAN_POINT('Ctrl Pts',(1.53209368873156,4.33500692163563,3.91799691542918));
#8677=CARTESIAN_POINT('Ctrl Pts',(1.53717057127463,4.33725843599311,3.88748431756648));
#8678=CARTESIAN_POINT('Ctrl Pts',(1.55076865302059,4.34470269924416,3.78741568145517));
#8679=CARTESIAN_POINT('Ctrl Pts',(1.55550000000259,4.35000710688228,3.71744083094467));
#8680=CARTESIAN_POINT('Ctrl Pts',(1.5555,4.35539415465377,3.64739446822635));
#8681=CARTESIAN_POINT('Origin',(-2.67773308947627E-16,1.2059437743963,3.64739446828387));
#8682=CARTESIAN_POINT('',(1.55549955406273,5.19405622556279,3.64857230980728));
#8683=CARTESIAN_POINT('',(1.5554999873946,5.05594377443822,3.64759249708933));
#8684=CARTESIAN_POINT('',(1.5555,1.2059437743963,3.64739446828386));
#8685=CARTESIAN_POINT('Ctrl Pts',(1.55549997006787,4.49405622566528,3.64769962209176));
#8686=CARTESIAN_POINT('Ctrl Pts',(1.5555112048523,4.49818264884198,3.59043110243972));
#8687=CARTESIAN_POINT('Ctrl Pts',(1.55235548796176,4.50230907201867,3.53303695693616));
#8688=CARTESIAN_POINT('Ctrl Pts',(1.54601728863953,4.50643549519536,3.47589871548611));
#8689=CARTESIAN_POINT('Ctrl Pts',(1.53969015520276,4.51055471403468,3.41886023190156));
#8690=CARTESIAN_POINT('Ctrl Pts',(1.53019162173891,4.514673932874,3.36207728507753));
#8691=CARTESIAN_POINT('Ctrl Pts',(1.51755815074409,4.51879315171333,3.30593069405566));
#8692=CARTESIAN_POINT('Ctrl Pts',(1.50493690032262,4.52290838596156,3.24983841459505));
#8693=CARTESIAN_POINT('Ctrl Pts',(1.48918683358188,4.52702362020979,3.19438178319573));
#8694=CARTESIAN_POINT('Ctrl Pts',(1.47039588386746,4.53113885445802,3.13993393316253));
#8695=CARTESIAN_POINT('Ctrl Pts',(1.45161569328146,4.53525173244781,3.08551725831847));
#8696=CARTESIAN_POINT('Ctrl Pts',(1.429798241767,4.53936461043761,3.03210871724348));
#8697=CARTESIAN_POINT('Ctrl Pts',(1.40508135769004,4.5434774884274,2.98006649174466));
#8698=CARTESIAN_POINT('Ctrl Pts',(1.38036886934147,4.54758963497004,2.92803352159889));
#8699=CARTESIAN_POINT('Ctrl Pts',(1.35275819858074,4.55170178151267,2.87736686006049));
#8700=CARTESIAN_POINT('Ctrl Pts',(1.32243444548008,4.55581392805531,2.8284027788219));
#8701=CARTESIAN_POINT('Ctrl Pts',(1.29208256946628,4.55992988829277,2.77939328722135));
#8702=CARTESIAN_POINT('Ctrl Pts',(1.25901286363791,4.56404584853022,2.73208997848173));
#8703=CARTESIAN_POINT('Ctrl Pts',(1.22345458874833,4.56816180876768,2.68680136021435));
#8704=CARTESIAN_POINT('Ctrl Pts',(1.18787941608737,4.5722797249649,2.64149122018531));
#8705=CARTESIAN_POINT('Ctrl Pts',(1.14981366757703,4.57639764116212,2.5981980734549));
#8706=CARTESIAN_POINT('Ctrl Pts',(1.10952573337371,4.58051555735934,2.55719590977192));
#8707=CARTESIAN_POINT('Ctrl Pts',(1.06916306124129,4.58464111268065,2.5161176831966));
#8708=CARTESIAN_POINT('Ctrl Pts',(1.02657036213311,4.58876666800197,2.47733928112318));
#8709=CARTESIAN_POINT('Ctrl Pts',(0.982050677732466,4.59289222332328,2.44109570082814));
#8710=CARTESIAN_POINT('Ctrl Pts',(0.951072578398685,4.59576290545572,2.41587635694225));
#8711=CARTESIAN_POINT('Ctrl Pts',(0.919162176237059,4.59863358758815,2.39188346783218));
#8712=CARTESIAN_POINT('Ctrl Pts',(0.886429325065603,4.60150426972059,2.36918349130717));
#8713=CARTESIAN_POINT('Ctrl Pts',(0.839127122506271,4.60565268890353,2.33637978343418));
#8714=CARTESIAN_POINT('Ctrl Pts',(0.789902466076941,4.60980110808647,2.30613665572483));
#8715=CARTESIAN_POINT('Ctrl Pts',(0.739063605726963,4.61394952726941,2.27868513585063));
#8716=CARTESIAN_POINT('Ctrl Pts',(0.688314982571474,4.61809058315376,2.25128234146162));
#8717=CARTESIAN_POINT('Ctrl Pts',(0.635958296846781,4.62223163903811,2.22666156523239));
#8718=CARTESIAN_POINT('Ctrl Pts',(0.582330668195567,4.62637269492246,2.20501059327732));
#8719=CARTESIAN_POINT('Ctrl Pts',(0.528756283717064,4.6305096393609,2.18338111748234));
#8720=CARTESIAN_POINT('Ctrl Pts',(0.473913936833557,4.63464658379933,2.16471579788028));
#8721=CARTESIAN_POINT('Ctrl Pts',(0.418163666519987,4.63878352823777,2.14915570293218));
#8722=CARTESIAN_POINT('Ctrl Pts',(0.362447327290461,4.64291795482277,2.13360507826801));
#8723=CARTESIAN_POINT('Ctrl Pts',(0.305824660527443,4.64705238140778,2.12115607155644));
#8724=CARTESIAN_POINT('Ctrl Pts',(0.248671830850362,4.65118680799278,2.11190022520071));
#8725=CARTESIAN_POINT('Ctrl Pts',(0.191531827588873,4.65532030671693,2.10264645607078));
#8726=CARTESIAN_POINT('Ctrl Pts',(0.133862411373075,4.65945380544108,2.09658450778817));
#8727=CARTESIAN_POINT('Ctrl Pts',(0.0760487419179381,4.66358730416522,2.09375460047258));
#8728=CARTESIAN_POINT('Ctrl Pts',(0.0181828671915226,4.66772453540495,2.09092213777379));
#8729=CARTESIAN_POINT('Ctrl Pts',(-0.0398269998096223,4.67186176664468,
2.09132757497707));
#8730=CARTESIAN_POINT('Ctrl Pts',(-0.0975931575225837,4.67599899788441,
2.09495901854537));
#8731=CARTESIAN_POINT('Ctrl Pts',(-0.155383239378268,4.68013794257913,2.09859196609416));
#8732=CARTESIAN_POINT('Ctrl Pts',(-0.212928892430087,4.68427688727384,2.10545352302032));
#8733=CARTESIAN_POINT('Ctrl Pts',(-0.269848249449828,4.68841583196855,2.11547992358209));
#8734=CARTESIAN_POINT('Ctrl Pts',(-0.326878241148675,4.69256282156823,2.12552581255109));
#8735=CARTESIAN_POINT('Ctrl Pts',(-0.383278995100198,4.69670981116791,2.13874871992923));
#8736=CARTESIAN_POINT('Ctrl Pts',(-0.438680449723717,4.70085680076759,2.15503401818135));
#8737=CARTESIAN_POINT('Ctrl Pts',(-0.490670975608389,4.70474847060895,2.17031667142701));
#8738=CARTESIAN_POINT('Ctrl Pts',(-0.541781273715216,4.7086401404503,2.18829563175241));
#8739=CARTESIAN_POINT('Ctrl Pts',(-0.591722488297608,4.71253181029166,2.20883798804304));
#8740=CARTESIAN_POINT('Ctrl Pts',(-0.644958489593133,4.71668022643349,2.23073559136017));
#8741=CARTESIAN_POINT('Ctrl Pts',(-0.69708881376828,4.72082864257532,2.25563816533533));
#8742=CARTESIAN_POINT('Ctrl Pts',(-0.747752051956195,4.72497705871715,2.28341238673173));
#8743=CARTESIAN_POINT('Ctrl Pts',(-0.798325364621596,4.7291181115616,2.31113730983097));
#8744=CARTESIAN_POINT('Ctrl Pts',(-0.84743630712596,4.73325916440605,2.34172351508062));
#8745=CARTESIAN_POINT('Ctrl Pts',(-0.894744095649219,4.7374002172505,2.37498995190519));
#8746=CARTESIAN_POINT('Ctrl Pts',(-0.942004914647774,4.74153715865178,2.40822336015719));
#8747=CARTESIAN_POINT('Ctrl Pts',(-0.987465702944342,4.74567410005306,2.44413142958445));
#8748=CARTESIAN_POINT('Ctrl Pts',(-1.03081245246944,4.74981104145434,2.48248849017493));
#8749=CARTESIAN_POINT('Ctrl Pts',(-1.07413282008242,4.75394546500998,2.52082220570235));
#8750=CARTESIAN_POINT('Ctrl Pts',(-1.11534131031366,4.75807988856562,2.5616016133837));
#8751=CARTESIAN_POINT('Ctrl Pts',(-1.15415673901441,4.76221431212126,2.60456060242238));
#8752=CARTESIAN_POINT('Ctrl Pts',(-1.19296345675003,4.76634780782886,2.6475099505974));
#8753=CARTESIAN_POINT('Ctrl Pts',(-1.22937783025491,4.77048130353646,2.6926375228735));
#8754=CARTESIAN_POINT('Ctrl Pts',(-1.26315688060045,4.77461479924406,2.73964177895062));
#8755=CARTESIAN_POINT('Ctrl Pts',(-1.29696643353523,4.77875202751135,2.78668848001956));
#8756=CARTESIAN_POINT('Ctrl Pts',(-1.32813560223634,4.78288925577863,2.83561482825171));
#8757=CARTESIAN_POINT('Ctrl Pts',(-1.35646378270186,4.78702648404592,2.88608884225832));
#8758=CARTESIAN_POINT('Ctrl Pts',(-1.38480369556457,4.79116542578737,2.93658376057894));
#8759=CARTESIAN_POINT('Ctrl Pts',(-1.41030004380524,4.79530436752882,2.98862715446294));
#8760=CARTESIAN_POINT('Ctrl Pts',(-1.4327989453742,4.79944330927028,3.04186376540037));
#8761=CARTESIAN_POINT('Ctrl Pts',(-1.45534157868286,4.80359029598771,3.09520385381669));
#8762=CARTESIAN_POINT('Ctrl Pts',(-1.474874945188,4.80773728270515,3.14974130245472));
#8763=CARTESIAN_POINT('Ctrl Pts',(-1.49129427990586,4.81188426942259,3.20510313814041));
#8764=CARTESIAN_POINT('Ctrl Pts',(-1.50670282295054,4.81577596323597,3.25705684045867));
#8765=CARTESIAN_POINT('Ctrl Pts',(-1.51936934366869,4.81966765704936,3.30973606651612));
#8766=CARTESIAN_POINT('Ctrl Pts',(-1.529248536561,4.82355935086274,3.36282608735225));
#8767=CARTESIAN_POINT('Ctrl Pts',(-1.53977943481766,4.82770776987243,3.41941832256457));
#8768=CARTESIAN_POINT('Ctrl Pts',(-1.54718672201664,4.83185618888211,3.47671443938883));
#8769=CARTESIAN_POINT('Ctrl Pts',(-1.55138603020248,4.8360046078918,3.53433857373343));
#8770=CARTESIAN_POINT('Ctrl Pts',(-1.55557788472731,4.84014566356742,3.59186042676303));
#8771=CARTESIAN_POINT('Ctrl Pts',(-1.55657302470185,4.84428671924304,3.64970862663675));
#8772=CARTESIAN_POINT('Ctrl Pts',(-1.55433835797629,4.84842777491866,3.70749870210799));
#8773=CARTESIAN_POINT('Ctrl Pts',(-1.55210590995044,4.85256471912704,3.7652314004221));
#8774=CARTESIAN_POINT('Ctrl Pts',(-1.54665002876785,4.85670166333542,3.82290557099127));
#8775=CARTESIAN_POINT('Ctrl Pts',(-1.53798962954333,4.8608386075438,3.88013498778397));
#8776=CARTESIAN_POINT('Ctrl Pts',(-1.52933450130965,4.86497303387807,3.93732957295701));
#8777=CARTESIAN_POINT('Ctrl Pts',(-1.51747879900516,4.86910746021233,3.99407942716118));
#8778=CARTESIAN_POINT('Ctrl Pts',(-1.50249322175679,4.87324188654659,4.05000391747117));
#8779=CARTESIAN_POINT('Ctrl Pts',(-1.48751100769123,4.87737538499991,4.10591585676088));
#8780=CARTESIAN_POINT('Ctrl Pts',(-1.46940044792973,4.88150888345323,4.16100229719957));
#8781=CARTESIAN_POINT('Ctrl Pts',(-1.44828274104248,4.88564238190655,4.21489543920681));
#8782=CARTESIAN_POINT('Ctrl Pts',(-1.42714596518474,4.88977961284657,4.26883724590764));
#8783=CARTESIAN_POINT('Ctrl Pts',(-1.40299680515486,4.89391684378659,4.32158311447313));
#8784=CARTESIAN_POINT('Ctrl Pts',(-1.37600503548616,4.89805407472661,4.3727842892193));
#8785=CARTESIAN_POINT('Ctrl Pts',(-1.34900208714668,4.90219301910532,4.42400666898771));
#8786=CARTESIAN_POINT('Ctrl Pts',(-1.31915444986938,4.90633196348404,4.47368263163852));
#8787=CARTESIAN_POINT('Ctrl Pts',(-1.28667682036272,4.91047090786275,4.52149000650683));
#8788=CARTESIAN_POINT('Ctrl Pts',(-1.25413606396406,4.9146178971234,4.56939030475151));
#8789=CARTESIAN_POINT('Ctrl Pts',(-1.21895541635321,4.91876488638404,4.61541434136025));
#8790=CARTESIAN_POINT('Ctrl Pts',(-1.18139112704005,4.92291187564469,4.65927156306913));
#8791=CARTESIAN_POINT('Ctrl Pts',(-1.1461395550944,4.9268035475744,4.70042863098323));
#8792=CARTESIAN_POINT('Ctrl Pts',(-1.10878944216815,4.93069521950411,4.73967755409274));
#8793=CARTESIAN_POINT('Ctrl Pts',(-1.06958042727821,4.93458689143382,4.77680934315642));
#8794=CARTESIAN_POINT('Ctrl Pts',(-1.02778460459304,4.93873531572807,4.81639089541027));
#8795=CARTESIAN_POINT('Ctrl Pts',(-0.983701114049857,4.94288374002232,4.85373212912806));
#8796=CARTESIAN_POINT('Ctrl Pts',(-0.937599712680937,4.94703216431657,4.88855804685868));
#8797=CARTESIAN_POINT('Ctrl Pts',(-0.891580139198416,4.95117322534676,4.92332215017249));
#8798=CARTESIAN_POINT('Ctrl Pts',(-0.843550176143913,4.95531428637694,4.95557948781596));
#8799=CARTESIAN_POINT('Ctrl Pts',(-0.79381465899519,4.95945534740713,4.9850934393399));
#8800=CARTESIAN_POINT('Ctrl Pts',(-0.74412852146618,4.96359229700889,5.01457808810825));
#8801=CARTESIAN_POINT('Ctrl Pts',(-0.692740630421603,4.96772924661066,5.04132448297697));
#8802=CARTESIAN_POINT('Ctrl Pts',(-0.63998554372013,4.97186619621242,5.06513871666905));
#8803=CARTESIAN_POINT('Ctrl Pts',(-0.58726256500489,4.97600062796938,5.08893845645854));
#8804=CARTESIAN_POINT('Ctrl Pts',(-0.533174513733451,4.98013505972634,5.1098093588572));
#8805=CARTESIAN_POINT('Ctrl Pts',(-0.478079379464037,4.9842694914833,5.1276040334912));
#8806=CARTESIAN_POINT('Ctrl Pts',(-0.422996609803048,4.9884029953792,5.14539471459317));
#8807=CARTESIAN_POINT('Ctrl Pts',(-0.366907701096103,4.9925364992751,5.16011037858373));
#8808=CARTESIAN_POINT('Ctrl Pts',(-0.310187297829203,4.996670003171,5.1716530061525));
#8809=CARTESIAN_POINT('Ctrl Pts',(-0.253415677140842,5.00080723954056,5.18320605648957));
#8810=CARTESIAN_POINT('Ctrl Pts',(-0.19601193360329,5.00494447591012,5.19158023947204));
#8811=CARTESIAN_POINT('Ctrl Pts',(-0.138361107359085,5.00908171227968,5.19672866527636));
#8812=CARTESIAN_POINT('Ctrl Pts',(-0.0806864049680436,5.01322066208979,
5.20187922330633));
#8813=CARTESIAN_POINT('Ctrl Pts',(-0.022764937357718,5.01735961189989,5.20380134227935));
#8814=CARTESIAN_POINT('Ctrl Pts',(0.0350161759650124,5.02149856170999,5.20250029022037));
#8815=CARTESIAN_POINT('Ctrl Pts',(0.0929095975521726,5.02564555633341,5.20119670932644));
#8816=CARTESIAN_POINT('Ctrl Pts',(0.150661598631048,5.02979255095683,5.19665747786724));
#8817=CARTESIAN_POINT('Ctrl Pts',(0.207889035770754,5.03393954558024,5.18893992619496));
#8818=CARTESIAN_POINT('Ctrl Pts',(0.261592491699019,5.03783117438846,5.18169760997704));
#8819=CARTESIAN_POINT('Ctrl Pts',(0.314833719845909,5.04172280319668,5.17165692314213));
#8820=CARTESIAN_POINT('Ctrl Pts',(0.367307093263549,5.0456144320049,5.15890554969819));
#8821=CARTESIAN_POINT('Ctrl Pts',(0.423242717723974,5.04976283477335,5.14531282657292));
#8822=CARTESIAN_POINT('Ctrl Pts',(0.478539950070272,5.05391123754181,5.12858247703888));
#8823=CARTESIAN_POINT('Ctrl Pts',(0.532821374524922,5.05805964031026,5.10879161924913));
#8824=CARTESIAN_POINT('Ctrl Pts',(0.587006451339249,5.0622006798081,5.08903588954357));
#8825=CARTESIAN_POINT('Ctrl Pts',(0.640178813855858,5.06634171930594,5.06623061086359));
#8826=CARTESIAN_POINT('Ctrl Pts',(0.691974214247196,5.07048275880377,5.04050319943768));
#8827=CARTESIAN_POINT('Ctrl Pts',(0.743718189736949,5.07461968688347,5.01480133139189));
#8828=CARTESIAN_POINT('Ctrl Pts',(0.794087447787117,5.07875661496317,4.98618330930379));
#8829=CARTESIAN_POINT('Ctrl Pts',(0.842737458631534,5.08289354304286,4.95482470574179));
#8830=CARTESIAN_POINT('Ctrl Pts',(0.891357860324589,5.08702795332395,4.92348518751241));
#8831=CARTESIAN_POINT('Ctrl Pts',(0.938260652246649,5.09116236360504,4.88940867573691));
#8832=CARTESIAN_POINT('Ctrl Pts',(0.983127633410276,5.09529677388613,4.8528156836377));
#8833=CARTESIAN_POINT('Ctrl Pts',(1.02798454623534,5.09943025638822,4.81623090315925));
#8834=CARTESIAN_POINT('Ctrl Pts',(1.07080615196489,5.10356373889032,4.7771310924156));
#8835=CARTESIAN_POINT('Ctrl Pts',(1.11130665585431,5.10769722139242,4.73577756565993));
#8836=CARTESIAN_POINT('Ctrl Pts',(1.1518437340318,5.11183443666732,4.6943866942874));
#8837=CARTESIAN_POINT('Ctrl Pts',(1.19005515556565,5.11597165194223,4.65073841184222));
#8838=CARTESIAN_POINT('Ctrl Pts',(1.2256924082796,5.12010886721714,4.60513053332776));
#8839=CARTESIAN_POINT('Ctrl Pts',(1.26134442137995,5.12424779606118,4.55950376475141));
#8840=CARTESIAN_POINT('Ctrl Pts',(1.29441984130309,5.12838672490521,4.5119162098285));
#8841=CARTESIAN_POINT('Ctrl Pts',(1.32471281917197,5.13252565374925,4.46269576027442));
#8842=CARTESIAN_POINT('Ctrl Pts',(1.35506468093426,5.13667262789824,4.41337963535565));
#8843=CARTESIAN_POINT('Ctrl Pts',(1.38262304284443,5.14081960204723,4.36242473206768));
#8844=CARTESIAN_POINT('Ctrl Pts',(1.40722792828634,5.14496657619622,4.3101838826916));
#8845=CARTESIAN_POINT('Ctrl Pts',(1.43031880371275,5.14885837498947,4.26115756440366));
#8846=CARTESIAN_POINT('Ctrl Pts',(1.45080881805183,5.15275017378272,4.21099922990207));
#8847=CARTESIAN_POINT('Ctrl Pts',(1.46860557248654,5.15664197257597,4.16001315938036));
#8848=CARTESIAN_POINT('Ctrl Pts',(1.490795582025,5.16149448951443,4.09644081559399));
#8849=CARTESIAN_POINT('Ctrl Pts',(1.50887543297797,5.16634700645289,4.03136398579588));
#8850=CARTESIAN_POINT('Ctrl Pts',(1.52267165228983,5.17119952339134,3.96528012274624));
#8851=CARTESIAN_POINT('Ctrl Pts',(1.53632980103551,5.17600347704257,3.89985761743379));
#8852=CARTESIAN_POINT('Ctrl Pts',(1.5457895385634,5.18080743069381,3.83344827699458));
#8853=CARTESIAN_POINT('Ctrl Pts',(1.5509290488956,5.18561138434504,3.76655543207561));
#8854=CARTESIAN_POINT('Ctrl Pts',(1.55394062032499,5.18842633141762,3.72735858888101));
#8855=CARTESIAN_POINT('Ctrl Pts',(1.55546970192271,5.19124127849021,3.68799611136951));
#8856=CARTESIAN_POINT('Ctrl Pts',(1.55549955406273,5.19405622556279,3.64857230980727));
#8857=CARTESIAN_POINT('Ctrl Pts',(1.5555,4.35539415465377,3.64739446822635));
#8858=CARTESIAN_POINT('Ctrl Pts',(1.55549999999998,4.35542999814836,3.64692840471078));
#8859=CARTESIAN_POINT('Ctrl Pts',(1.55549979055613,4.35546584504022,3.6464623380092));
#8860=CARTESIAN_POINT('Ctrl Pts',(1.55542473595912,4.36188857679378,3.56296395502293));
#8861=CARTESIAN_POINT('Ctrl Pts',(1.54870199287245,4.36837449542619,3.48007311827894));
#8862=CARTESIAN_POINT('Ctrl Pts',(1.52889270440882,4.37785809760788,3.35806064973547));
#8863=CARTESIAN_POINT('Ctrl Pts',(1.52082399216785,4.38093859904206,3.31827147924465));
#8864=CARTESIAN_POINT('Ctrl Pts',(1.50684734298435,4.38531873479868,3.26096210660124));
#8865=CARTESIAN_POINT('Ctrl Pts',(1.5021700412061,4.3866710431493,3.24316169155459));
#8866=CARTESIAN_POINT('Ctrl Pts',(1.49307977307113,4.38910145249918,3.21090706305395));
#8867=CARTESIAN_POINT('Ctrl Pts',(1.48877062776986,4.39018445434306,3.19642827795496));
#8868=CARTESIAN_POINT('Ctrl Pts',(1.47714668947669,4.39294051384069,3.15935583138254));
#8869=CARTESIAN_POINT('Ctrl Pts',(1.46952431871862,4.39459689997359,3.13686289014809));
#8870=CARTESIAN_POINT('Ctrl Pts',(1.45091238522665,4.39833868534909,3.0858172824324));
#8871=CARTESIAN_POINT('Ctrl Pts',(1.43958953000541,4.40040948261442,3.05739624327111));
#8872=CARTESIAN_POINT('Ctrl Pts',(1.3935987134821,4.40816645041638,2.95118001327726));
#8873=CARTESIAN_POINT('Ctrl Pts',(1.35340098778299,4.41370528325842,2.87594199554569));
#8874=CARTESIAN_POINT('Ctrl Pts',(1.27096408468862,4.42377475954,2.74811029532056));
#8875=CARTESIAN_POINT('Ctrl Pts',(1.23109277753004,4.428255456671,2.6942571150238));
#8876=CARTESIAN_POINT('Ctrl Pts',(1.1680043673741,4.43498426132566,2.61963291254187));
#8877=CARTESIAN_POINT('Ctrl Pts',(1.14743635971125,4.43712901503914,2.59671964265142));
#8878=CARTESIAN_POINT('Ctrl Pts',(1.10833588627034,4.44113146877616,2.55567895097275));
#8879=CARTESIAN_POINT('Ctrl Pts',(1.09000387279488,4.44298009405443,2.53737527190501));
#8880=CARTESIAN_POINT('Ctrl Pts',(1.04684672837064,4.4472756489092,2.49638511099435));
#8881=CARTESIAN_POINT('Ctrl Pts',(1.02172668075684,4.44973562529083,2.47402970038339));
#8882=CARTESIAN_POINT('Ctrl Pts',(0.938928703210333,4.45772661735186,2.40501999259121));
#8883=CARTESIAN_POINT('Ctrl Pts',(0.878637787054446,4.46337778056003,2.36167507033747));
#8884=CARTESIAN_POINT('Ctrl Pts',(0.726626581277196,4.47715923622267,2.26808858605383));
#8885=CARTESIAN_POINT('Ctrl Pts',(0.632476451274895,4.48533743175628,2.2224570852839));
#8886=CARTESIAN_POINT('Ctrl Pts',(0.51389604740648,4.49479424411113,2.17907206156493));
#8887=CARTESIAN_POINT('Ctrl Pts',(0.493171773749558,4.49641661501248,2.1719821285031));
#8888=CARTESIAN_POINT('Ctrl Pts',(0.458079326012494,4.49910532165137,2.16079887788345));
#8889=CARTESIAN_POINT('Ctrl Pts',(0.44379066473939,4.50018369446635,2.15647091884479));
#8890=CARTESIAN_POINT('Ctrl Pts',(0.410678268950601,4.50264447935619,2.14695964673775));
#8891=CARTESIAN_POINT('Ctrl Pts',(0.391815574230482,4.50401897428642,2.14192379497555));
#8892=CARTESIAN_POINT('Ctrl Pts',(0.313977050032271,4.50959855783355,2.12270516721571));
#8893=CARTESIAN_POINT('Ctrl Pts',(0.254285161224476,4.51366228573275,2.11162111071004));
#8894=CARTESIAN_POINT('Ctrl Pts',(0.0684829468289144,4.52606993601891,2.08825446455554));
#8895=CARTESIAN_POINT('Ctrl Pts',(-0.0585741758224798,4.5342576646857,2.08785139797022));
#8896=CARTESIAN_POINT('Ctrl Pts',(-0.216408854516841,4.54516460934817,2.1066820276763));
#8897=CARTESIAN_POINT('Ctrl Pts',(-0.248414344754627,4.54741203071616,2.11151762772879));
#8898=CARTESIAN_POINT('Ctrl Pts',(-0.305677513142983,4.55151215067336,2.12200596710727));
#8899=CARTESIAN_POINT('Ctrl Pts',(-0.330989559564697,4.5533527030844,2.12729756806451));
#8900=CARTESIAN_POINT('Ctrl Pts',(-0.387127098001552,4.55750396918868,2.14050193863259));
#8901=CARTESIAN_POINT('Ctrl Pts',(-0.417864477660436,4.55982431334066,2.14873457099195));
#8902=CARTESIAN_POINT('Ctrl Pts',(-0.482454373697825,4.56480659263543,2.16817565209562));
#8903=CARTESIAN_POINT('Ctrl Pts',(-0.516217209066973,4.56747461720144,2.17961724720742));
#8904=CARTESIAN_POINT('Ctrl Pts',(-0.616455924361088,4.57558649949667,2.21747265391306));
#8905=CARTESIAN_POINT('Ctrl Pts',(-0.681529451947081,4.5811157931353,2.24731936958475));
#8906=CARTESIAN_POINT('Ctrl Pts',(-0.810726560539948,4.5925232712912,2.31772414450078));
#8907=CARTESIAN_POINT('Ctrl Pts',(-0.87441706813729,4.59838835464249,2.35871396976759));
#8908=CARTESIAN_POINT('Ctrl Pts',(-0.952591794174984,4.60571793002098,2.41749999648646));
#8909=CARTESIAN_POINT('Ctrl Pts',(-0.97002144512225,4.60736081083441,2.43119955320827));
#8910=CARTESIAN_POINT('Ctrl Pts',(-0.998705307251497,4.61007133987632,2.45475395708422));
#8911=CARTESIAN_POINT('Ctrl Pts',(-1.01012003536558,4.61115155011968,2.46440619165219));
#8912=CARTESIAN_POINT('Ctrl Pts',(-1.03597528651205,4.6136011516674,2.48691648062338));
#8913=CARTESIAN_POINT('Ctrl Pts',(-1.05031825667497,4.61496302755117,2.49988167554502));
#8914=CARTESIAN_POINT('Ctrl Pts',(-1.10646622025366,4.62032447951741,2.5525712094774));
#8915=CARTESIAN_POINT('Ctrl Pts',(-1.14629392514209,4.62419688080577,2.59434309080453));
#8916=CARTESIAN_POINT('Ctrl Pts',(-1.25460414204208,4.63527457122279,2.72138768445489));
#8917=CARTESIAN_POINT('Ctrl Pts',(-1.31653308385251,4.64235106796483,2.8117747636599));
#8918=CARTESIAN_POINT('Ctrl Pts',(-1.38824632396734,4.65255069316582,2.94448532693523));
#8919=CARTESIAN_POINT('Ctrl Pts',(-1.40653715151324,4.65539975421856,2.98184066910839));
#8920=CARTESIAN_POINT('Ctrl Pts',(-1.43413299580547,4.66017171477297,3.04443282191966));
#8921=CARTESIAN_POINT('Ctrl Pts',(-1.44431966234323,4.66206380018973,3.06925888761211));
#8922=CARTESIAN_POINT('Ctrl Pts',(-1.46370230015254,4.66595323500559,3.12021109068446));
#8923=CARTESIAN_POINT('Ctrl Pts',(-1.47285268958301,4.66795131216819,3.14634406304927));
#8924=CARTESIAN_POINT('Ctrl Pts',(-1.4957746290852,4.67343547084167,3.21787363350106));
#8925=CARTESIAN_POINT('Ctrl Pts',(-1.50817388211601,4.67696409985088,3.26367508107682));
#8926=CARTESIAN_POINT('Ctrl Pts',(-1.53299545183572,4.68561167185927,3.37537493216633));
#8927=CARTESIAN_POINT('Ctrl Pts',(-1.54328759819419,4.69077900636863,3.44164798915467));
#8928=CARTESIAN_POINT('Ctrl Pts',(-1.55672745150483,4.70243354335533,3.591422803953));
#8929=CARTESIAN_POINT('Ctrl Pts',(-1.5574904033563,4.70891850701704,3.6749445312974));
#8930=CARTESIAN_POINT('Ctrl Pts',(-1.54998777875069,4.7168131069242,3.78006612871679));
#8931=CARTESIAN_POINT('Ctrl Pts',(-1.5479570642334,4.7184425982157,3.80196789962133));
#8932=CARTESIAN_POINT('Ctrl Pts',(-1.54376846267121,4.72113885910744,3.83865930334746));
#8933=CARTESIAN_POINT('Ctrl Pts',(-1.54186089649022,4.72221784814295,3.85347296396247));
#8934=CARTESIAN_POINT('Ctrl Pts',(-1.53697778997546,4.72467463794818,3.88751518709492));
#8935=CARTESIAN_POINT('Ctrl Pts',(-1.5338544371308,4.72604466352001,3.90671926351459));
#8936=CARTESIAN_POINT('Ctrl Pts',(-1.51971159811976,4.73154357133582,3.9844442386269));
#8937=CARTESIAN_POINT('Ctrl Pts',(-1.5056953768279,4.73553644040192,4.04237414377839));
#8938=CARTESIAN_POINT('Ctrl Pts',(-1.44985041264986,4.74827744764488,4.22627853082451));
#8939=CARTESIAN_POINT('Ctrl Pts',(-1.39524132686724,4.75684396019484,4.34773184749127));
#8940=CARTESIAN_POINT('Ctrl Pts',(-1.30981470610301,4.76809456482178,4.48698395210403));
#8941=CARTESIAN_POINT('Ctrl Pts',(-1.2929695035071,4.77023620124597,4.51270059951141));
#8942=CARTESIAN_POINT('Ctrl Pts',(-1.26054325591555,4.7742358831103,4.55914120380146));
#8943=CARTESIAN_POINT('Ctrl Pts',(-1.24518448300833,4.77608494904194,4.58000739144719));
#8944=CARTESIAN_POINT('Ctrl Pts',(-1.20867120393973,4.78038602871796,4.62710313544392));
#8945=CARTESIAN_POINT('Ctrl Pts',(-1.18717188668116,4.78285121678727,4.65304735908694));
#8946=CARTESIAN_POINT('Ctrl Pts',(-1.11570732639708,4.7908467590375,4.73379938693622));
#8947=CARTESIAN_POINT('Ctrl Pts',(-1.06266489891863,4.79649695392724,4.78573496557076));
#8948=CARTESIAN_POINT('Ctrl Pts',(-0.926709698403657,4.81026035894515,4.90104268528015));
#8949=CARTESIAN_POINT('Ctrl Pts',(-0.840724536636249,4.81842067398266,4.96025739752718));
#8950=CARTESIAN_POINT('Ctrl Pts',(-0.730244834359119,4.82786399248016,5.02100422202298));
#8951=CARTESIAN_POINT('Ctrl Pts',(-0.710803484380253,4.82948889400623,5.03116461320231));
#8952=CARTESIAN_POINT('Ctrl Pts',(-0.677776337640811,4.8321802833817,5.04754532419139));
#8953=CARTESIAN_POINT('Ctrl Pts',(-0.664305236812612,4.8332588731138,5.05398673398091));
#8954=CARTESIAN_POINT('Ctrl Pts',(-0.63303328058106,4.8357182275306,5.06839032584697));
#8955=CARTESIAN_POINT('Ctrl Pts',(-0.61517199606121,4.83709112577514,5.07621351721705));
#8956=CARTESIAN_POINT('Ctrl Pts',(-0.541533940049074,4.84264138873306,5.1068297425127));
#8957=CARTESIAN_POINT('Ctrl Pts',(-0.484597085563224,4.84667935041719,5.12671108817259));
#8958=CARTESIAN_POINT('Ctrl Pts',(-0.300022473846509,4.8593987841055,5.179355346805));
#8959=CARTESIAN_POINT('Ctrl Pts',(-0.169339690549315,4.86790736886002,5.19924479353335));
#8960=CARTESIAN_POINT('Ctrl Pts',(-0.00693726053703426,4.87909349000794,
5.20318365165234));
#8961=CARTESIAN_POINT('Ctrl Pts',(0.0238543599284254,4.88123833983494,5.20301616049979));
#8962=CARTESIAN_POINT('Ctrl Pts',(0.0805057286813397,4.88524087923301,5.20102570800575));
#8963=CARTESIAN_POINT('Ctrl Pts',(0.106364194731054,4.88708949112897,5.19946975994246));
#8964=CARTESIAN_POINT('Ctrl Pts',(0.165667618915032,4.89138487683024,5.19441247539608));
#8965=CARTESIAN_POINT('Ctrl Pts',(0.199060825190142,4.89384469353514,5.19047092059296));
#8966=CARTESIAN_POINT('Ctrl Pts',(0.305636727207883,4.90183554276984,5.17437440333785));
#8967=CARTESIAN_POINT('Ctrl Pts',(0.378079556000965,4.90748673212127,5.15806804776789));
#8968=CARTESIAN_POINT('Ctrl Pts',(0.548996000259684,4.92126877416249,5.10652976367326));
#8969=CARTESIAN_POINT('Ctrl Pts',(0.645635091687667,4.92944755621753,5.06641872758857));
#8970=CARTESIAN_POINT('Ctrl Pts',(0.756812690538516,4.93890481289353,5.00654653594583));
#8971=CARTESIAN_POINT('Ctrl Pts',(0.775873061328148,4.94052710273782,4.99575677770474));
#8972=CARTESIAN_POINT('Ctrl Pts',(0.807533810189901,4.94321572188394,4.97694035353649));
#8973=CARTESIAN_POINT('Ctrl Pts',(0.820256839427936,4.94429408624312,4.96912889660789));
#8974=CARTESIAN_POINT('Ctrl Pts',(0.849354163985706,4.94675490993549,4.95068216686474));
#8975=CARTESIAN_POINT('Ctrl Pts',(0.865644040164713,4.94812945060267,4.93991983166864));
#8976=CARTESIAN_POINT('Ctrl Pts',(0.931705492617353,4.95370991074706,4.89446519351761));
#8977=CARTESIAN_POINT('Ctrl Pts',(0.979634465981861,4.95777441024533,4.85717896516727));
#8978=CARTESIAN_POINT('Ctrl Pts',(1.12045677245441,4.9701812864885,4.73375460362749));
#8979=CARTESIAN_POINT('Ctrl Pts',(1.2050998194748,4.97836762238755,4.63902655933112));
#8980=CARTESIAN_POINT('Ctrl Pts',(1.29580110506019,4.98927315414945,4.50851427377775));
#8981=CARTESIAN_POINT('Ctrl Pts',(1.31343668563415,4.99152078286865,4.4813678702151));
#8982=CARTESIAN_POINT('Ctrl Pts',(1.34361465959424,4.9956211066508,4.43158096879652));
#8983=CARTESIAN_POINT('Ctrl Pts',(1.35646337366098,4.99746164930446,4.40913969473083));
#8984=CARTESIAN_POINT('Ctrl Pts',(1.38385985427357,5.00161266991114,4.35839671230256));
#8985=CARTESIAN_POINT('Ctrl Pts',(1.39811010021698,5.00393277247568,4.32994861158317));
#8986=CARTESIAN_POINT('Ctrl Pts',(1.45176048803832,5.01336249309508,4.21410442814453));
#8987=CARTESIAN_POINT('Ctrl Pts',(1.48391078081463,5.0207068912447,4.12360010393777));
#8988=CARTESIAN_POINT('Ctrl Pts',(1.5287126263025,5.03479064832996,3.94740938413806));
#8989=CARTESIAN_POINT('Ctrl Pts',(1.54295667978206,5.04148626376499,3.86247127854805));
#8990=CARTESIAN_POINT('Ctrl Pts',(1.55196051596764,5.04960547706827,3.75460553906682));
#8991=CARTESIAN_POINT('Ctrl Pts',(1.5533358305926,5.05125710375816,3.73238618335164));
#8992=CARTESIAN_POINT('Ctrl Pts',(1.55469402656414,5.05371899289713,3.69874495057206));
#8993=CARTESIAN_POINT('Ctrl Pts',(1.55502884006779,5.05454679470241,3.6873410315443));
#8994=CARTESIAN_POINT('Ctrl Pts',(1.55541087755945,5.05604459048751,3.66652198520036));
#8995=CARTESIAN_POINT('Ctrl Pts',(1.55549815372627,5.05671690269938,3.6571086182568));
#8996=CARTESIAN_POINT('Ctrl Pts',(1.55549997101641,5.05738485701522,3.64769474805265));
#8997=CARTESIAN_POINT('Origin',(-2.67773308947627E-16,1.2059437743963,3.64739446828387));
#8998=CARTESIAN_POINT('',(1.55549964733824,5.89405622564623,3.64634702825329));
#8999=CARTESIAN_POINT('',(1.5554995134887,5.7559437743963,3.64862472695888));
#9000=CARTESIAN_POINT('',(1.5555,1.2059437743963,3.64739446828386));
#9001=CARTESIAN_POINT('Ctrl Pts',(1.55549955406316,5.1940562256037,3.64857230923438));
#9002=CARTESIAN_POINT('Ctrl Pts',(1.55554339101516,5.19818989105023,3.59067963768888));
#9003=CARTESIAN_POINT('Ctrl Pts',(1.55235092862268,5.20232355649676,3.53275114493701));
#9004=CARTESIAN_POINT('Ctrl Pts',(1.54593674727678,5.20645722194329,3.47517419241811));
#9005=CARTESIAN_POINT('Ctrl Pts',(1.53952345737511,5.21059031289216,3.4176052419557));
#9006=CARTESIAN_POINT('Ctrl Pts',(1.52988939577038,5.21472340384103,3.36038825123378));
#9007=CARTESIAN_POINT('Ctrl Pts',(1.51710097035125,5.2188564947899,3.30390517331344));
#9008=CARTESIAN_POINT('Ctrl Pts',(1.50429938807024,5.2229938379047,3.24736398502915));
#9009=CARTESIAN_POINT('Ctrl Pts',(1.48833707342149,5.22713118101949,3.19155872648236));
#9010=CARTESIAN_POINT('Ctrl Pts',(1.46933126780937,5.23126852413429,3.13685957678506));
#9011=CARTESIAN_POINT('Ctrl Pts',(1.4503162406771,5.23540787466691,3.08213388733872));
#9012=CARTESIAN_POINT('Ctrl Pts',(1.42825497839268,5.23954722519952,3.02851585791755));
#9013=CARTESIAN_POINT('Ctrl Pts',(1.40331301745104,5.24368657573214,2.97635585162128));
#9014=CARTESIAN_POINT('Ctrl Pts',(1.37832001504554,5.24783439707068,2.92408910459671));
#9015=CARTESIAN_POINT('Ctrl Pts',(1.35043478546577,5.25198221840923,2.87328680009967));
#9016=CARTESIAN_POINT('Ctrl Pts',(1.31986857258952,5.25613003974777,2.82427406330627));
#9017=CARTESIAN_POINT('Ctrl Pts',(1.29152292864674,5.25997653088087,2.77882199531761));
#9018=CARTESIAN_POINT('Ctrl Pts',(1.26087236047473,5.26382302201396,2.73490888339637));
#9019=CARTESIAN_POINT('Ctrl Pts',(1.22811608950117,5.26766951314705,2.69276830024302));
#9020=CARTESIAN_POINT('Ctrl Pts',(1.1927883306997,5.27181796799075,2.64731952621754));
#9021=CARTESIAN_POINT('Ctrl Pts',(1.15486031021853,5.27596642283445,2.60373928251711));
#9022=CARTESIAN_POINT('Ctrl Pts',(1.11455708914475,5.28011487767815,2.56234020925477));
#9023=CARTESIAN_POINT('Ctrl Pts',(1.07432540113556,5.28425596954489,2.52101461405456));
#9024=CARTESIAN_POINT('Ctrl Pts',(1.03172724032223,5.28839706141163,2.48186287528167));
#9025=CARTESIAN_POINT('Ctrl Pts',(0.987028147397972,5.29253815327837,2.44516500339619));
#9026=CARTESIAN_POINT('Ctrl Pts',(0.942373431723652,5.29667513386998,2.4085035651501));
#9027=CARTESIAN_POINT('Ctrl Pts',(0.89562231697053,5.30081211446159,2.37429149565244));
#9028=CARTESIAN_POINT('Ctrl Pts',(0.847076184934661,5.30494909505321,2.34277107936409));
#9029=CARTESIAN_POINT('Ctrl Pts',(0.798559597826388,5.3090835578996,2.31126984623983));
#9030=CARTESIAN_POINT('Ctrl Pts',(0.748250594795294,5.31321802074599,2.28245730203282));
#9031=CARTESIAN_POINT('Ctrl Pts',(0.696480755874186,5.31735248359238,2.25653329379631));
#9032=CARTESIAN_POINT('Ctrl Pts',(0.644722534624885,5.32148601862378,2.23061510316761));
#9033=CARTESIAN_POINT('Ctrl Pts',(0.591504593667746,5.32561955365519,2.20758439462339));
#9034=CARTESIAN_POINT('Ctrl Pts',(0.537182444298231,5.32975308868659,2.18759473149194));
#9035=CARTESIAN_POINT('Ctrl Pts',(0.48281124580911,5.3338903560124,2.16758701908613));
#9036=CARTESIAN_POINT('Ctrl Pts',(0.427334335914796,5.33802762333821,2.15062602066201));
#9037=CARTESIAN_POINT('Ctrl Pts',(0.37112523597503,5.34216489066401,2.1368163308734));
#9038=CARTESIAN_POINT('Ctrl Pts',(0.314892857790601,5.34630387138358,2.12300092198704));
#9039=CARTESIAN_POINT('Ctrl Pts',(0.257928197727324,5.35044285210315,2.11233952072553));
#9040=CARTESIAN_POINT('Ctrl Pts',(0.20061472232642,5.35458183282272,2.10488547862258));
#9041=CARTESIAN_POINT('Ctrl Pts',(0.14318985516695,5.35872885786934,2.09741694919614));
#9042=CARTESIAN_POINT('Ctrl Pts',(0.0854153389819498,5.36287588291597,2.09316827547533));
#9043=CARTESIAN_POINT('Ctrl Pts',(0.0276785853041187,5.36702290796259,2.09214074431612));
#9044=CARTESIAN_POINT('Ctrl Pts',(-0.0264989894077483,5.37091428988111,
2.09117655525801));
#9045=CARTESIAN_POINT('Ctrl Pts',(-0.0806429526473259,5.37480567179962,
2.09304809442987));
#9046=CARTESIAN_POINT('Ctrl Pts',(-0.134437993166186,5.37869705371814,2.0977149285101));
#9047=CARTESIAN_POINT('Ctrl Pts',(-0.191784778467867,5.38284535886403,2.10268988399774));
#9048=CARTESIAN_POINT('Ctrl Pts',(-0.248975180305849,5.38699366400992,2.11086278502762));
#9049=CARTESIAN_POINT('Ctrl Pts',(-0.305624474969962,5.39114196915581,2.12221450175555));
#9050=CARTESIAN_POINT('Ctrl Pts',(-0.362173217818001,5.39528291111001,2.13354606932294));
#9051=CARTESIAN_POINT('Ctrl Pts',(-0.418182253502629,5.3994238530642,2.14804515179915));
#9052=CARTESIAN_POINT('Ctrl Pts',(-0.473272264851127,5.4035647950184,2.16564090803079));
#9053=CARTESIAN_POINT('Ctrl Pts',(-0.528307580459116,5.40770162566673,2.18321919443635));
#9054=CARTESIAN_POINT('Ctrl Pts',(-0.582425186030991,5.41183845631507,2.20388790541525));
#9055=CARTESIAN_POINT('Ctrl Pts',(-0.635257970069161,5.4159752869634,2.2275256146697));
#9056=CARTESIAN_POINT('Ctrl Pts',(-0.688058601996187,5.42010960008704,2.25114893887387));
#9057=CARTESIAN_POINT('Ctrl Pts',(-0.739575487986166,5.42424391321067,2.27773746746318));
#9058=CARTESIAN_POINT('Ctrl Pts',(-0.789460743674072,5.42837822633431,2.30712136768176));
#9059=CARTESIAN_POINT('Ctrl Pts',(-0.839334809894685,5.43251161211456,2.33649867697111));
#9060=CARTESIAN_POINT('Ctrl Pts',(-0.887577523941612,5.43664499789482,2.36866984892289));
#9061=CARTESIAN_POINT('Ctrl Pts',(-0.933866862659667,5.44077838367508,2.40341981708466));
#9062=CARTESIAN_POINT('Ctrl Pts',(-0.980198020559222,5.44491550368043,2.43820117941334));
#9063=CARTESIAN_POINT('Ctrl Pts',(-1.024571858391,5.44905262368578,2.47556568122309));
#9064=CARTESIAN_POINT('Ctrl Pts',(-1.06669768505826,5.45318974369113,2.51525653556924));
#9065=CARTESIAN_POINT('Ctrl Pts',(-1.10884096645356,5.45732857790152,2.55496383571891));
#9066=CARTESIAN_POINT('Ctrl Pts',(-1.14873401962118,5.46146741211192,2.59699903237818));
#9067=CARTESIAN_POINT('Ctrl Pts',(-1.18612377654658,5.46560624632231,2.64106915472424));
#9068=CARTESIAN_POINT('Ctrl Pts',(-1.2235862347266,5.46975312814961,2.68522496773667));
#9069=CARTESIAN_POINT('Ctrl Pts',(-1.25853535357741,5.4739000099769,2.73142319730467));
#9070=CARTESIAN_POINT('Ctrl Pts',(-1.29075963708497,5.4780468918042,2.77933928036534));
#9071=CARTESIAN_POINT('Ctrl Pts',(-1.32100771353262,5.48193945929921,2.82431683101129));
#9072=CARTESIAN_POINT('Ctrl Pts',(-1.34885515567857,5.48583202679421,2.8708074098687));
#9073=CARTESIAN_POINT('Ctrl Pts',(-1.37416452409191,5.48972459428922,2.91852403348268));
#9074=CARTESIAN_POINT('Ctrl Pts',(-1.40113808296194,5.49387311339754,2.96937821265902));
#9075=CARTESIAN_POINT('Ctrl Pts',(-1.42534134831133,5.49802163250586,3.02183823319597));
#9076=CARTESIAN_POINT('Ctrl Pts',(-1.44658140734488,5.50217015161417,3.07557064758022));
#9077=CARTESIAN_POINT('Ctrl Pts',(-1.46778375951885,5.50631130597707,3.12920767237065));
#9078=CARTESIAN_POINT('Ctrl Pts',(-1.48603315695587,5.51045246033997,3.18411212726837));
#9079=CARTESIAN_POINT('Ctrl Pts',(-1.50118304248143,5.51459361470287,3.23992701809158));
#9080=CARTESIAN_POINT('Ctrl Pts',(-1.51631788336419,5.51873065667904,3.29568648175705));
#9081=CARTESIAN_POINT('Ctrl Pts',(-1.52835917507792,5.52286769865521,3.3523540900666));
#9082=CARTESIAN_POINT('Ctrl Pts',(-1.53720946298209,5.52700474063138,3.40955562175469));
#9083=CARTESIAN_POINT('Ctrl Pts',(-1.54605436215694,5.53113926366132,3.46672232479381));
#9084=CARTESIAN_POINT('Ctrl Pts',(-1.55171202954512,5.53527378669126,3.52442179328072));
#9085=CARTESIAN_POINT('Ctrl Pts',(-1.5541360973046,5.5394083097212,3.58226965692273));
#9086=CARTESIAN_POINT('Ctrl Pts',(-1.55655962032951,5.54354190364442,3.64010452103892));
#9087=CARTESIAN_POINT('Ctrl Pts',(-1.55575096456502,5.54767549756764,3.69808719414853));
#9088=CARTESIAN_POINT('Ctrl Pts',(-1.5517157883933,5.55180909149086,3.75583044963211));
#9089=CARTESIAN_POINT('Ctrl Pts',(-1.54767697120438,5.55594641523552,3.81362580796767));
#9090=CARTESIAN_POINT('Ctrl Pts',(-1.54040585086494,5.56008373898018,3.87118079622946));
#9091=CARTESIAN_POINT('Ctrl Pts',(-1.52996013383856,5.56422106272484,3.92811183302054));
#9092=CARTESIAN_POINT('Ctrl Pts',(-1.51951009409349,5.56836009860536,3.98506642940604));
#9093=CARTESIAN_POINT('Ctrl Pts',(-1.5058829600887,5.57249913448588,4.04139605210123));
#9094=CARTESIAN_POINT('Ctrl Pts',(-1.48918725521303,5.57663817036639,4.09672905287655));
#9095=CARTESIAN_POINT('Ctrl Pts',(-1.47245911320342,5.58078524774395,4.15216955698707));
#9096=CARTESIAN_POINT('Ctrl Pts',(-1.4526506642247,5.5849323251215,4.20660907835336));
#9097=CARTESIAN_POINT('Ctrl Pts',(-1.42991953843312,5.58907940249905,4.25969371179738));
#9098=CARTESIAN_POINT('Ctrl Pts',(-1.40859252316599,5.59297031328613,4.3094992866858));
#9099=CARTESIAN_POINT('Ctrl Pts',(-1.38469337269005,5.59686122407321,4.35811207240156));
#9100=CARTESIAN_POINT('Ctrl Pts',(-1.35838814834895,5.6007521348603,4.40526113757677));
#9101=CARTESIAN_POINT('Ctrl Pts',(-1.33034059139179,5.60490076102295,4.45553313198483));
#9102=CARTESIAN_POINT('Ctrl Pts',(-1.29943983349395,5.6090493871856,4.5043512258202));
#9103=CARTESIAN_POINT('Ctrl Pts',(-1.26586108932038,5.61319801334825,4.55137231787126));
#9104=CARTESIAN_POINT('Ctrl Pts',(-1.2323419222398,5.61733927881018,4.59830998274113));
#9105=CARTESIAN_POINT('Ctrl Pts',(-1.19615449993241,5.6214805442721,4.64345655405963));
#9106=CARTESIAN_POINT('Ctrl Pts',(-1.15751898488021,5.62562180973402,4.68649506478158));
#9107=CARTESIAN_POINT('Ctrl Pts',(-1.11892181377584,5.629758965183,4.72949086178772));
#9108=CARTESIAN_POINT('Ctrl Pts',(-1.07788170981581,5.63389612063199,4.77038235794144));
#9109=CARTESIAN_POINT('Ctrl Pts',(-1.03465996895199,5.63803327608097,4.80888445904929));
#9110=CARTESIAN_POINT('Ctrl Pts',(-0.991464521539586,5.64216791473878,4.84736313784457));
#9111=CARTESIAN_POINT('Ctrl Pts',(-0.946090456058851,5.64630255339659,4.88345495740179));
#9112=CARTESIAN_POINT('Ctrl Pts',(-0.898835336805198,5.6504371920544,4.91691220636802));
#9113=CARTESIAN_POINT('Ctrl Pts',(-0.851590814222675,5.65457090354481,4.95036195275104));
#9114=CARTESIAN_POINT('Ctrl Pts',(-0.802466500010218,5.65870461503523,4.98117800074386));
#9115=CARTESIAN_POINT('Ctrl Pts',(-0.751790614076356,5.66283832652564,5.00915477119577));
#9116=CARTESIAN_POINT('Ctrl Pts',(-0.701068978425304,5.66697576989223,5.03715679881511));
#9117=CARTESIAN_POINT('Ctrl Pts',(-0.648793428175893,5.67111321325882,5.06231417327492));
#9118=CARTESIAN_POINT('Ctrl Pts',(-0.595317392221518,5.67525065662541,5.08446699690536));
#9119=CARTESIAN_POINT('Ctrl Pts',(-0.54181921002405,5.67938981344785,5.10662899477261));
#9120=CARTESIAN_POINT('Ctrl Pts',(-0.487120043010132,5.68352897027029,5.12578378759072));
#9121=CARTESIAN_POINT('Ctrl Pts',(-0.431590901758725,5.68766812709273,5.1418206268876));
#9122=CARTESIAN_POINT('Ctrl Pts',(-0.375953871087437,5.69181532602096,5.15788862469422));
#9123=CARTESIAN_POINT('Ctrl Pts',(-0.31948415272831,5.69596252494919,5.17082644518591));
#9124=CARTESIAN_POINT('Ctrl Pts',(-0.262564532221247,5.70010972387742,5.18057420869901));
#9125=CARTESIAN_POINT('Ctrl Pts',(-0.209175146173626,5.70399970772874,5.1897174022879));
#9126=CARTESIAN_POINT('Ctrl Pts',(-0.155390369769416,5.70788969158005,5.19605443380858));
#9127=CARTESIAN_POINT('Ctrl Pts',(-0.10152764302057,5.71177967543137,5.19957757207758));
#9128=CARTESIAN_POINT('Ctrl Pts',(-0.0440976842286706,5.71592728595477,
5.20333404149196));
#9129=CARTESIAN_POINT('Ctrl Pts',(0.0136615881029582,5.72007489647816,5.20390677509005));
#9130=CARTESIAN_POINT('Ctrl Pts',(0.0713670981046381,5.72422250700156,5.20125642718116));
#9131=CARTESIAN_POINT('Ctrl Pts',(0.1289701615635,5.72836275413177,5.19861078452452));
#9132=CARTESIAN_POINT('Ctrl Pts',(0.186519136065157,5.73250300126198,5.1927534414133));
#9133=CARTESIAN_POINT('Ctrl Pts',(0.24362845718739,5.73664324839219,5.18369698564446));
#9134=CARTESIAN_POINT('Ctrl Pts',(0.300681072802416,5.74077938455052,5.17464952229416));
#9135=CARTESIAN_POINT('Ctrl Pts',(0.357294388064168,5.74491552070884,5.16240932097463));
#9136=CARTESIAN_POINT('Ctrl Pts',(0.413087244050112,5.74905165686716,5.14704081952908));
#9137=CARTESIAN_POINT('Ctrl Pts',(0.468846160906999,5.75318527698905,5.13168166683518));
#9138=CARTESIAN_POINT('Ctrl Pts',(0.523785106630126,5.75731889711093,5.11319812425796));
#9139=CARTESIAN_POINT('Ctrl Pts',(0.577534600719311,5.76145251723282,5.09170538874802));
#9140=CARTESIAN_POINT('Ctrl Pts',(0.631272070913041,5.7655852126536,5.07021746121644));
#9141=CARTESIAN_POINT('Ctrl Pts',(0.683820134277734,5.76971790807439,5.045721870491));
#9142=CARTESIAN_POINT('Ctrl Pts',(0.734828029057464,5.77385060349518,5.01838243967951));
#9143=CARTESIAN_POINT('Ctrl Pts',(0.785882132555134,5.77798704277871,4.99101824172064));
#9144=CARTESIAN_POINT('Ctrl Pts',(0.835392818450878,5.78212348206224,4.960805301017));
#9145=CARTESIAN_POINT('Ctrl Pts',(0.883033984203594,5.78625992134577,4.92795342153106));
#9146=CARTESIAN_POINT('Ctrl Pts',(0.930694940833089,5.79039807897013,4.89508789486649));
#9147=CARTESIAN_POINT('Ctrl Pts',(0.976484415800411,5.79453623659449,4.85958156294093));
#9148=CARTESIAN_POINT('Ctrl Pts',(1.02010802560609,5.79867439421885,4.82168568688939));
#9149=CARTESIAN_POINT('Ctrl Pts',(1.0638166387669,5.80282061530434,4.7837159683332));
#9150=CARTESIAN_POINT('Ctrl Pts',(1.10535057742059,5.80696683638983,4.74334776458119));
#9151=CARTESIAN_POINT('Ctrl Pts',(1.14445177490565,5.81111305747533,4.70086985238894));
#9152=CARTESIAN_POINT('Ctrl Pts',(1.18121260623956,5.8150111103177,4.66093441649563));
#9153=CARTESIAN_POINT('Ctrl Pts',(1.21582333906809,5.81890916316007,4.61913487527535));
#9154=CARTESIAN_POINT('Ctrl Pts',(1.24810396751098,5.82280721600245,4.57573531963284));
#9155=CARTESIAN_POINT('Ctrl Pts',(1.28262086856108,5.82697531032832,4.52932921665439));
#9156=CARTESIAN_POINT('Ctrl Pts',(1.31461877168976,5.83114340465419,4.48089784141524));
#9157=CARTESIAN_POINT('Ctrl Pts',(1.34385418886972,5.83531149898005,4.43074379588766));
#9158=CARTESIAN_POINT('Ctrl Pts',(1.37304289061388,5.8394729330848,4.38066989178852));
#9159=CARTESIAN_POINT('Ctrl Pts',(1.39947760178787,5.84363436718955,4.3288792150418));
#9160=CARTESIAN_POINT('Ctrl Pts',(1.42295681421145,5.8477958012943,4.27570502436996));
#9161=CARTESIAN_POINT('Ctrl Pts',(1.4464053075886,5.8519517907834,4.22260040419319));
#9162=CARTESIAN_POINT('Ctrl Pts',(1.46690577030673,5.85610778027249,4.16811633035345));
#9163=CARTESIAN_POINT('Ctrl Pts',(1.48430262546914,5.86026376976159,4.11261051059691));
#9164=CARTESIAN_POINT('Ctrl Pts',(1.50168590311237,5.86441651567439,4.05714801081549));
#9165=CARTESIAN_POINT('Ctrl Pts',(1.51597022498911,5.86856926158719,4.00066583607904));
#9166=CARTESIAN_POINT('Ctrl Pts',(1.52704887102887,5.87272200749999,3.94353969530846));
#9167=CARTESIAN_POINT('Ctrl Pts',(1.53812567839228,5.87687406419899,3.88642303552353));
#9168=CARTESIAN_POINT('Ctrl Pts',(1.54599775636003,5.881026120898,3.82866312385785));
#9169=CARTESIAN_POINT('Ctrl Pts',(1.5506092566561,5.885178177597,3.77064698619895));
#9170=CARTESIAN_POINT('Ctrl Pts',(1.55389607119802,5.88813752693257,3.72929639036671));
#9171=CARTESIAN_POINT('Ctrl Pts',(1.55552757156221,5.89109687626813,3.68781588946909));
#9172=CARTESIAN_POINT('Ctrl Pts',(1.55549964733864,5.8940562256037,3.64634702884922));
#9173=CARTESIAN_POINT('Ctrl Pts',(1.5554999873946,5.05594377443823,3.64759249708933));
#9174=CARTESIAN_POINT('Ctrl Pts',(1.55550729033478,5.06007749260067,3.59022850230281));
#9175=CARTESIAN_POINT('Ctrl Pts',(1.55233707856484,5.06421121076312,3.53274024496008));
#9176=CARTESIAN_POINT('Ctrl Pts',(1.54597416002809,5.06834492892557,3.47551036045119));
#9177=CARTESIAN_POINT('Ctrl Pts',(1.53962245335763,5.07247136321427,3.41838131863089));
#9178=CARTESIAN_POINT('Ctrl Pts',(1.5300892612969,5.07659779750297,3.36151026343843));
#9179=CARTESIAN_POINT('Ctrl Pts',(1.51741138191812,5.08072423179167,3.30527906666428));
#9180=CARTESIAN_POINT('Ctrl Pts',(1.50474592422412,5.08484662303307,3.24910296476678));
#9181=CARTESIAN_POINT('Ctrl Pts',(1.48894199726885,5.08896901427447,3.19356598886568));
#9182=CARTESIAN_POINT('Ctrl Pts',(1.47008786542628,5.09309140551588,3.13904230892344));
#9183=CARTESIAN_POINT('Ctrl Pts',(1.45124482651563,5.09721137132577,3.08455070828747));
#9184=CARTESIAN_POINT('Ctrl Pts',(1.42935531067883,5.10133133713567,3.03107171707727));
#9185=CARTESIAN_POINT('Ctrl Pts',(1.40455747949938,5.10545130294556,2.97896456411864));
#9186=CARTESIAN_POINT('Ctrl Pts',(1.37976453193656,5.10957045738073,2.92686767299931));
#9187=CARTESIAN_POINT('Ctrl Pts',(1.35206463182601,5.1136896118159,2.87614255733828));
#9188=CARTESIAN_POINT('Ctrl Pts',(1.3216432290437,5.11780876625106,2.82712656989765));
#9189=CARTESIAN_POINT('Ctrl Pts',(1.29119393642363,5.12193169705873,2.7780656454123));
#9190=CARTESIAN_POINT('Ctrl Pts',(1.25801843387563,5.1260546278664,2.7307174264883));
#9191=CARTESIAN_POINT('Ctrl Pts',(1.22234637900804,5.13017755867407,2.68539156822279));
#9192=CARTESIAN_POINT('Ctrl Pts',(1.18665819797229,5.13430235332377,2.64004521962066));
#9193=CARTESIAN_POINT('Ctrl Pts',(1.14847156347857,5.13842714797348,2.59672344769715));
#9194=CARTESIAN_POINT('Ctrl Pts',(1.10805533127371,5.14255194262319,2.55570145610695));
#9195=CARTESIAN_POINT('Ctrl Pts',(1.06756285499791,5.14668451858052,2.514602077698));
#9196=CARTESIAN_POINT('Ctrl Pts',(1.02483276916788,5.15081709453785,2.47581149899184));
#9197=CARTESIAN_POINT('Ctrl Pts',(0.980168736436743,5.15494967049518,2.43956604581982));
#9198=CARTESIAN_POINT('Ctrl Pts',(0.945182812488144,5.15818677156542,2.41117450590241));
#9199=CARTESIAN_POINT('Ctrl Pts',(0.909010995181922,5.16142387263566,2.38434383327528));
#9200=CARTESIAN_POINT('Ctrl Pts',(0.87181086109517,5.16466097370589,2.35916852828868));
#9201=CARTESIAN_POINT('Ctrl Pts',(0.824137977463899,5.16880939807082,2.32690575788551));
#9202=CARTESIAN_POINT('Ctrl Pts',(0.77457193097481,5.17295782243575,2.29722530939668));
#9203=CARTESIAN_POINT('Ctrl Pts',(0.723423584422977,5.17710624680067,2.27035468399998));
#9204=CARTESIAN_POINT('Ctrl Pts',(0.672366023848988,5.18124730790192,2.24353175273548));
#9205=CARTESIAN_POINT('Ctrl Pts',(0.61973219489561,5.18538836900317,2.21950898557959));
#9206=CARTESIAN_POINT('Ctrl Pts',(0.565861335505652,5.18952943010441,2.19847031603167));
#9207=CARTESIAN_POINT('Ctrl Pts',(0.512043961482645,5.19366637977742,2.17745253460348));
#9208=CARTESIAN_POINT('Ctrl Pts',(0.456992472997552,5.19780332945043,2.15941316913124));
#9209=CARTESIAN_POINT('Ctrl Pts',(0.401068493576888,5.20194027912344,2.14448917736898));
#9210=CARTESIAN_POINT('Ctrl Pts',(0.345178550803582,5.20607471095171,2.12957426869863));
#9211=CARTESIAN_POINT('Ctrl Pts',(0.288417671795299,5.21020914277998,2.11777110909836));
#9212=CARTESIAN_POINT('Ctrl Pts',(0.231163040437577,5.21434357460825,2.10916694976275));
#9213=CARTESIAN_POINT('Ctrl Pts',(0.173921258329439,5.2184770785754,2.1005647213974));
#9214=CARTESIAN_POINT('Ctrl Pts',(0.116186458521773,5.22261058254255,2.09516014532916));
#9215=CARTESIAN_POINT('Ctrl Pts',(0.0583442347286331,5.2267440865097,2.09298905132408));
#9216=CARTESIAN_POINT('Ctrl Pts',(0.000449780542036197,5.23088132294985,
2.09081599686371));
#9217=CARTESIAN_POINT('Ctrl Pts',(-0.0575517699355378,5.23501855939,2.09188227998785));
#9218=CARTESIAN_POINT('Ctrl Pts',(-0.115272874994606,5.23915579583016,2.09617159123155));
#9219=CARTESIAN_POINT('Ctrl Pts',(-0.173017885302765,5.24329474571061,2.10046267889747));
#9220=CARTESIAN_POINT('Ctrl Pts',(-0.230481701072578,5.24743369559106,2.10797938931007));
#9221=CARTESIAN_POINT('Ctrl Pts',(-0.287283205457954,5.25157264547151,2.11865361062951));
#9222=CARTESIAN_POINT('Ctrl Pts',(-0.344195114036731,5.25571964016395,2.12934857926554));
#9223=CARTESIAN_POINT('Ctrl Pts',(-0.400441631037956,5.25986663485638,2.14321319915192));
#9224=CARTESIAN_POINT('Ctrl Pts',(-0.455654023891854,5.26401362954881,2.16012863444274));
#9225=CARTESIAN_POINT('Ctrl Pts',(-0.507466510599438,5.26790525779153,2.17600243959509));
#9226=CARTESIAN_POINT('Ctrl Pts',(-0.558368129507022,5.27179688603425,2.19456229161848));
#9227=CARTESIAN_POINT('Ctrl Pts',(-0.608071567144028,5.27568851427696,2.21567200242989));
#9228=CARTESIAN_POINT('Ctrl Pts',(-0.661054498308607,5.27983691690472,2.23817455774595));
#9229=CARTESIAN_POINT('Ctrl Pts',(-0.712897604072605,5.28398531953248,2.26366927627782));
#9230=CARTESIAN_POINT('Ctrl Pts',(-0.763241019271799,5.28813372216024,2.29201872831324));
#9231=CARTESIAN_POINT('Ctrl Pts',(-0.813495076661055,5.2922747615177,2.32031786105789));
#9232=CARTESIAN_POINT('Ctrl Pts',(-0.86225427703073,5.29641580087517,2.35146141648696));
#9233=CARTESIAN_POINT('Ctrl Pts',(-0.909179922442212,5.30055684023263,2.38526447552244));
#9234=CARTESIAN_POINT('Ctrl Pts',(-0.956058977874828,5.30469376817225,2.41903397329749));
#9235=CARTESIAN_POINT('Ctrl Pts',(-1.00110766483905,5.30883069611187,2.45545744026071));
#9236=CARTESIAN_POINT('Ctrl Pts',(-1.04401456758374,5.31296762405148,2.49430564574116));
#9237=CARTESIAN_POINT('Ctrl Pts',(-1.08689535652621,5.317102034193,2.53313020760509));
#9238=CARTESIAN_POINT('Ctrl Pts',(-1.12763656001698,5.32123644433453,2.57437623387093));
#9239=CARTESIAN_POINT('Ctrl Pts',(-1.16596004471818,5.32537085447605,2.61777442957018));
#9240=CARTESIAN_POINT('Ctrl Pts',(-1.20427492947551,5.32950433683933,2.66116288654003));
#9241=CARTESIAN_POINT('Ctrl Pts',(-1.24017282806981,5.33363781920261,2.70670216401744));
#9242=CARTESIAN_POINT('Ctrl Pts',(-1.27341421348183,5.33777130156589,2.75408797502276));
#9243=CARTESIAN_POINT('Ctrl Pts',(-1.30668561779893,5.34190851670424,2.80151657817242));
#9244=CARTESIAN_POINT('Ctrl Pts',(-1.3372954141674,5.34604573184259,2.85079462055183));
#9245=CARTESIAN_POINT('Ctrl Pts',(-1.36504679451197,5.35018294698094,2.90158785877133));
#9246=CARTESIAN_POINT('Ctrl Pts',(-1.39280966904651,5.35432187568943,2.95240213475981));
#9247=CARTESIAN_POINT('Ctrl Pts',(-1.41771154198753,5.35846080439793,3.00473238704087));
#9248=CARTESIAN_POINT('Ctrl Pts',(-1.43960258938021,5.36259973310642,3.05822162891514));
#9249=CARTESIAN_POINT('Ctrl Pts',(-1.4615361889018,5.36674670712333,3.11181484393767));
#9250=CARTESIAN_POINT('Ctrl Pts',(-1.48044709586664,5.37089368114024,3.16657105698246));
#9251=CARTESIAN_POINT('Ctrl Pts',(-1.49623480202499,5.37504065515716,3.22211612741844));
#9252=CARTESIAN_POINT('Ctrl Pts',(-1.51105104947427,5.37893245505412,3.27424336489757));
#9253=CARTESIAN_POINT('Ctrl Pts',(-1.52311703828431,5.38282425495108,3.3270648830507));
#9254=CARTESIAN_POINT('Ctrl Pts',(-1.53239104897987,5.38671605484804,3.3802654301649));
#9255=CARTESIAN_POINT('Ctrl Pts',(-1.54227659502676,5.39086448300385,3.43697406200514));
#9256=CARTESIAN_POINT('Ctrl Pts',(-1.54903070265896,5.39501291115965,3.49435094749466));
#9257=CARTESIAN_POINT('Ctrl Pts',(-1.55257329113124,5.39916133931545,3.55201928458328));
#9258=CARTESIAN_POINT('Ctrl Pts',(-1.55610959145807,5.40330240395166,3.60958525954484));
#9259=CARTESIAN_POINT('Ctrl Pts',(-1.55644565569209,5.40744346858788,3.66744114383862));
#9260=CARTESIAN_POINT('Ctrl Pts',(-1.55355277362111,5.41158453322409,3.72520211298642));
#9261=CARTESIAN_POINT('Ctrl Pts',(-1.55066276383851,5.41572148627485,3.78290573235077));
#9262=CARTESIAN_POINT('Ctrl Pts',(-1.54455018566779,5.41985843932562,3.84051410586874));
#9263=CARTESIAN_POINT('Ctrl Pts',(-1.53523835277222,5.42399539237639,3.89764124683908));
#9264=CARTESIAN_POINT('Ctrl Pts',(-1.52593218763453,5.42812982742145,3.9547336166953));
#9265=CARTESIAN_POINT('Ctrl Pts',(-1.51343071143483,5.43226426246652,4.01134482177342));
#9266=CARTESIAN_POINT('Ctrl Pts',(-1.49780895477391,5.43639869751158,4.06709505798932));
#9267=CARTESIAN_POINT('Ctrl Pts',(-1.48219070461306,5.44053220453062,4.1228327803624));
#9268=CARTESIAN_POINT('Ctrl Pts',(-1.46345370489614,5.44466571154965,4.1777094164092));
#9269=CARTESIAN_POINT('Ctrl Pts',(-1.44172333621145,5.44879921856869,4.23135856976901));
#9270=CARTESIAN_POINT('Ctrl Pts',(-1.41997334691544,5.45293645778094,4.28505616359482));
#9271=CARTESIAN_POINT('Ctrl Pts',(-1.39522478243097,5.4570736969932,4.33752357571357));
#9272=CARTESIAN_POINT('Ctrl Pts',(-1.36765137923411,5.46121093620545,4.38841400573146));
#9273=CARTESIAN_POINT('Ctrl Pts',(-1.3400665574826,5.46534988870974,4.43932551023016));
#9274=CARTESIAN_POINT('Ctrl Pts',(-1.3096548376794,5.46948884121402,4.48865828586489));
#9275=CARTESIAN_POINT('Ctrl Pts',(-1.27663457277853,5.47362779371831,4.53609262715818));
#9276=CARTESIAN_POINT('Ctrl Pts',(-1.24355012920008,5.47777479075219,4.58361916254213));
#9277=CARTESIAN_POINT('Ctrl Pts',(-1.20784733002482,5.48192178778608,4.62923947777169));
#9278=CARTESIAN_POINT('Ctrl Pts',(-1.16978571820343,5.48606878481996,4.67266595598227));
#9279=CARTESIAN_POINT('Ctrl Pts',(-1.13406813706516,5.48996038835301,4.71341800732246));
#9280=CARTESIAN_POINT('Ctrl Pts',(-1.09627396077845,5.49385199188607,4.75223819906194));
#9281=CARTESIAN_POINT('Ctrl Pts',(-1.05664517948853,5.49774359541912,4.78892029570244));
#9282=CARTESIAN_POINT('Ctrl Pts',(-1.01440083906866,5.50189205063471,4.82802346585696));
#9283=CARTESIAN_POINT('Ctrl Pts',(-0.969894475223351,5.50604050585029,4.8648603570922));
#9284=CARTESIAN_POINT('Ctrl Pts',(-0.923398966675603,5.51018896106588,4.8991590621043));
#9285=CARTESIAN_POINT('Ctrl Pts',(-0.876985981675346,5.51433005330703,4.93339689132646));
#9286=CARTESIAN_POINT('Ctrl Pts',(-0.82859127507044,5.51847114554817,4.96510516952084));
#9287=CARTESIAN_POINT('Ctrl Pts',(-0.778522364130129,5.52261223778932,4.99405076390991));
#9288=CARTESIAN_POINT('Ctrl Pts',(-0.728503161574028,5.52674921875662,5.02296762113054));
#9289=CARTESIAN_POINT('Ctrl Pts',(-0.676813496421531,5.53088619972392,5.04912696958259));
#9290=CARTESIAN_POINT('Ctrl Pts',(-0.623790119403965,5.53502318069121,5.07233872576694));
#9291=CARTESIAN_POINT('Ctrl Pts',(-0.570799012131173,5.53915764391393,5.09553635540014));
#9292=CARTESIAN_POINT('Ctrl Pts',(-0.516476278018669,5.54329210713666,5.11578974041624));
#9293=CARTESIAN_POINT('Ctrl Pts',(-0.461181567724967,5.54742657035938,5.13295557829946));
#9294=CARTESIAN_POINT('Ctrl Pts',(-0.405899266118428,5.55156010576712,5.15011756399662));
#9295=CARTESIAN_POINT('Ctrl Pts',(-0.349645918398432,5.55569364117485,5.1641932238359));
#9296=CARTESIAN_POINT('Ctrl Pts',(-0.292797266397992,5.55982717658259,5.17508881297127));
#9297=CARTESIAN_POINT('Ctrl Pts',(-0.235897284068059,5.56396444428172,5.18599424005637));
#9298=CARTESIAN_POINT('Ctrl Pts',(-0.178401435691084,5.56810171198085,5.19371375896985));
#9299=CARTESIAN_POINT('Ctrl Pts',(-0.120695275443355,5.57223897967997,5.19820486948888));
#9300=CARTESIAN_POINT('Ctrl Pts',(-0.0629652169800224,5.57637796077183,
5.2026978399398));
#9301=CARTESIAN_POINT('Ctrl Pts',(-0.00502519466757172,5.58051694186369,
5.2039597239652));
#9302=CARTESIAN_POINT('Ctrl Pts',(0.0527377522754739,5.58465592295555,5.20200019948549));
#9303=CARTESIAN_POINT('Ctrl Pts',(0.110612964446322,5.58880294836786,5.20003686657021));
#9304=CARTESIAN_POINT('Ctrl Pts',(0.168309892939886,5.59294997378016,5.19483965925701));
#9305=CARTESIAN_POINT('Ctrl Pts',(0.225446067434111,5.59709699919247,5.18647026910672));
#9306=CARTESIAN_POINT('Ctrl Pts',(0.279060039765969,5.60098837812505,5.17861681626491));
#9307=CARTESIAN_POINT('Ctrl Pts',(0.332179991546601,5.60487975705762,5.16797080129299));
#9308=CARTESIAN_POINT('Ctrl Pts',(0.384501375266136,5.6087711359902,5.15462336344825));
#9309=CARTESIAN_POINT('Ctrl Pts',(0.440277239262835,5.61291944031003,5.14039467099007));
#9310=CARTESIAN_POINT('Ctrl Pts',(0.495379075984238,5.61706774462986,5.12303596400893));
#9311=CARTESIAN_POINT('Ctrl Pts',(0.549430385440946,5.62121604894968,5.10262864241332));
#9312=CARTESIAN_POINT('Ctrl Pts',(0.603385754467325,5.62535699007876,5.08225754357041));
#9313=CARTESIAN_POINT('Ctrl Pts',(0.656293814205358,5.62949793120784,5.05884875313529));
#9314=CARTESIAN_POINT('Ctrl Pts',(0.707791803327991,5.63363887233692,5.03253381619862));
#9315=CARTESIAN_POINT('Ctrl Pts',(0.759238663028474,5.63777570216126,5.006245005865));
#9316=CARTESIAN_POINT('Ctrl Pts',(0.809277764542756,5.64191253198559,4.97705600153326));
#9317=CARTESIAN_POINT('Ctrl Pts',(0.857566610935065,5.64604936180993,4.94514627730181));
#9318=CARTESIAN_POINT('Ctrl Pts',(0.905826070514475,5.65018367411204,4.91325597215295));
#9319=CARTESIAN_POINT('Ctrl Pts',(0.952336952841351,5.65431798641414,4.87864851575008));
#9320=CARTESIAN_POINT('Ctrl Pts',(0.996783599410229,5.65845229871625,4.8415480203645));
#9321=CARTESIAN_POINT('Ctrl Pts',(1.04122027645305,5.66258568367879,4.80445584673959));
#9322=CARTESIAN_POINT('Ctrl Pts',(1.08359323739862,5.66671906864133,4.7648720778326));
#9323=CARTESIAN_POINT('Ctrl Pts',(1.12361969242522,5.67085245360386,4.72306125534864));
#9324=CARTESIAN_POINT('Ctrl Pts',(1.16368230868329,5.67498957280393,4.68121265957627));
#9325=CARTESIAN_POINT('Ctrl Pts',(1.20139382085382,5.67912669200399,4.6371333657748));
#9326=CARTESIAN_POINT('Ctrl Pts',(1.23650913495829,5.68326381120405,4.59112398947344));
#9327=CARTESIAN_POINT('Ctrl Pts',(1.27163899905214,5.68740264461462,4.54509554924077));
#9328=CARTESIAN_POINT('Ctrl Pts',(1.30417022656156,5.69154147802519,4.49713586336888));
#9329=CARTESIAN_POINT('Ctrl Pts',(1.33390072694397,5.69568031143576,4.44757513579487));
#9330=CARTESIAN_POINT('Ctrl Pts',(1.36368903594959,5.69982719248287,4.39791804127818));
#9331=CARTESIAN_POINT('Ctrl Pts',(1.39066549083344,5.70397407352997,4.34665414594402));
#9332=CARTESIAN_POINT('Ctrl Pts',(1.41467415468491,5.70812095457708,4.29413806977254));
#9333=CARTESIAN_POINT('Ctrl Pts',(1.4372104897027,5.71201352857181,4.24484253655411));
#9334=CARTESIAN_POINT('Ctrl Pts',(1.45713220257539,5.71590610256655,4.19444423214131));
#9335=CARTESIAN_POINT('Ctrl Pts',(1.47435032060801,5.71979867656128,4.14324866270301));
#9336=CARTESIAN_POINT('Ctrl Pts',(1.49606381173456,5.72470753888491,4.07868675526277));
#9337=CARTESIAN_POINT('Ctrl Pts',(1.51355274598842,5.72961640120853,4.01263698113696));
#9338=CARTESIAN_POINT('Ctrl Pts',(1.52664550808754,5.73452526353215,3.94561207781779));
#9339=CARTESIAN_POINT('Ctrl Pts',(1.53959353558512,5.73937986058868,3.879328104686));
#9340=CARTESIAN_POINT('Ctrl Pts',(1.54824196854562,5.7442344576452,3.81209054589745));
#9341=CARTESIAN_POINT('Ctrl Pts',(1.55247128364616,5.74908905470172,3.74441592701353));
#9342=CARTESIAN_POINT('Ctrl Pts',(1.55446188960699,5.75137396126658,3.71256360659188));
#9343=CARTESIAN_POINT('Ctrl Pts',(1.55547421228667,5.75365886783144,3.68061475333113));
#9344=CARTESIAN_POINT('Ctrl Pts',(1.5554995134887,5.7559437743963,3.64862472695888));
#9345=CARTESIAN_POINT('Origin',(-2.67773308947627E-16,1.2059437743963,3.64739446828387));
#9346=CARTESIAN_POINT('',(1.55549999978821,6.5940562256037,3.64736879997355));
#9347=CARTESIAN_POINT('',(1.55498804050902,6.4559437743963,3.64654572419703));
#9348=CARTESIAN_POINT('',(1.5555,1.2059437743963,3.64739446828386));
#9349=CARTESIAN_POINT('Ctrl Pts',(1.55549964733824,5.89405622564623,3.64634702825329));
#9350=CARTESIAN_POINT('Ctrl Pts',(1.55545520190131,5.8987664550661,3.58034338179295));
#9351=CARTESIAN_POINT('Ctrl Pts',(1.5512056609363,5.90347668448598,3.51450400917047));
#9352=CARTESIAN_POINT('Ctrl Pts',(1.54283758956271,5.90818691390586,3.44932270797381));
#9353=CARTESIAN_POINT('Ctrl Pts',(1.53439597916476,5.91293853705441,3.38356859028426));
#9354=CARTESIAN_POINT('Ctrl Pts',(1.5217632534121,5.91769016020297,3.31848438005986));
#9355=CARTESIAN_POINT('Ctrl Pts',(1.50507796139441,5.92244178335153,3.25455788632538));
#9356=CARTESIAN_POINT('Ctrl Pts',(1.49174251234781,5.9262394410922,3.20346567295443));
#9357=CARTESIAN_POINT('Ctrl Pts',(1.47581937761426,5.93003709883287,3.15311264217503));
#9358=CARTESIAN_POINT('Ctrl Pts',(1.4574010096598,5.93383475657353,3.10373782384495));
#9359=CARTESIAN_POINT('Ctrl Pts',(1.43727628109979,5.93798424644059,3.0497886998482));
#9360=CARTESIAN_POINT('Ctrl Pts',(1.41410998760309,5.94213373630765,2.99684609065117));
#9361=CARTESIAN_POINT('Ctrl Pts',(1.38802361564244,5.94628322617471,2.94527575152801));
#9362=CARTESIAN_POINT('Ctrl Pts',(1.36198340764074,5.95042537286349,2.89379667427224));
#9363=CARTESIAN_POINT('Ctrl Pts',(1.33303361120312,5.95456751955227,2.84368550740763));
#9364=CARTESIAN_POINT('Ctrl Pts',(1.30134408932062,5.95870966624105,2.79528895181876));
#9365=CARTESIAN_POINT('Ctrl Pts',(1.26968593451922,5.96284771292947,2.74694030035068));
#9366=CARTESIAN_POINT('Ctrl Pts',(1.2352937110507,5.9669857596179,2.70030333063741));
#9367=CARTESIAN_POINT('Ctrl Pts',(1.1983827542823,5.97112380630632,2.65569944246254));
#9368=CARTESIAN_POINT('Ctrl Pts',(1.16149417217826,5.97525934459577,2.61112259224915));
#9369=CARTESIAN_POINT('Ctrl Pts',(1.1220902145225,5.97939488288523,2.56857678059709));
#9370=CARTESIAN_POINT('Ctrl Pts',(1.08042771304446,5.98353042117469,2.52835192803551));
#9371=CARTESIAN_POINT('Ctrl Pts',(1.03877448374495,5.98766503908135,2.48813602769717));
#9372=CARTESIAN_POINT('Ctrl Pts',(0.994864082749182,5.99179965698802,2.45024042219376));
#9373=CARTESIAN_POINT('Ctrl Pts',(0.948990009129902,5.99593427489469,2.41491801310445));
#9374=CARTESIAN_POINT('Ctrl Pts',(0.903074494523561,6.00007262786636,2.37956369502206));
#9375=CARTESIAN_POINT('Ctrl Pts',(0.855192174987022,6.00421098083804,2.34678753775245));
#9376=CARTESIAN_POINT('Ctrl Pts',(0.805668371193128,6.00834933380971,2.31680109476249));
#9377=CARTESIAN_POINT('Ctrl Pts',(0.756124023673007,6.01248940347485,2.28680221263765));
#9378=CARTESIAN_POINT('Ctrl Pts',(0.704937294292784,6.01662947314,2.2595955977478));
#9379=CARTESIAN_POINT('Ctrl Pts',(0.652458312882739,6.02076954280514,2.23534687703554));
#9380=CARTESIAN_POINT('Ctrl Pts',(0.599877475057094,6.02491764792839,2.21105109199946));
#9381=CARTESIAN_POINT('Ctrl Pts',(0.5459998582304,6.02906575305163,2.18972486694803));
#9382=CARTESIAN_POINT('Ctrl Pts',(0.491194922589105,6.03321385817488,2.17148532540865));
#9383=CARTESIAN_POINT('Ctrl Pts',(0.439895037533934,6.03709667116479,2.15441229405699));
#9384=CARTESIAN_POINT('Ctrl Pts',(0.387783153444932,6.0409794841547,2.14004335041999));
#9385=CARTESIAN_POINT('Ctrl Pts',(0.335170067944931,6.04486229714461,2.12843387776357));
#9386=CARTESIAN_POINT('Ctrl Pts',(0.279034259797698,6.04900508487512,2.11604708988489));
#9387=CARTESIAN_POINT('Ctrl Pts',(0.22209136397401,6.05314787260562,2.10675003836955));
#9388=CARTESIAN_POINT('Ctrl Pts',(0.164713239438893,6.05729066033612,2.10063986630153));
#9389=CARTESIAN_POINT('Ctrl Pts',(0.107437185811349,6.06142607839208,2.09454056372103));
#9390=CARTESIAN_POINT('Ctrl Pts',(0.0497279550305338,6.06556149644804,2.09161694391283));
#9391=CARTESIAN_POINT('Ctrl Pts',(-0.00803220328827441,6.06969691450401,
2.09191520654158));
#9392=CARTESIAN_POINT('Ctrl Pts',(-0.0657349316439698,6.07382822078269,
2.09221317261277));
#9393=CARTESIAN_POINT('Ctrl Pts',(-0.123487967648636,6.07795952706138,2.09572667211675));
#9394=CARTESIAN_POINT('Ctrl Pts',(-0.180905515729008,6.08209083334007,2.10244998889996));
#9395=CARTESIAN_POINT('Ctrl Pts',(-0.238288194124668,6.08621963067589,2.10916922261198));
#9396=CARTESIAN_POINT('Ctrl Pts',(-0.295335270781317,6.09034842801172,2.11909434928145));
#9397=CARTESIAN_POINT('Ctrl Pts',(-0.351664776387442,6.09447722534754,2.13216770801055));
#9398=CARTESIAN_POINT('Ctrl Pts',(-0.407981870661645,6.09860511296698,2.14523818622805));
#9399=CARTESIAN_POINT('Ctrl Pts',(-0.463581199258403,6.10273300058642,2.16145540146297));
#9400=CARTESIAN_POINT('Ctrl Pts',(-0.518091919598055,6.10686088820586,2.18071078976038));
#9401=CARTESIAN_POINT('Ctrl Pts',(-0.572652892458911,6.11099258125585,2.19998392927815));
#9402=CARTESIAN_POINT('Ctrl Pts',(-0.626122757588664,6.11512427430583,2.22230066550838));
#9403=CARTESIAN_POINT('Ctrl Pts',(-0.678148079973918,6.11925596735582,2.24750324692855));
#9404=CARTESIAN_POINT('Ctrl Pts',(-0.730195361219324,6.12338940431177,2.27271646586013));
#9405=CARTESIAN_POINT('Ctrl Pts',(-0.780796426362216,6.12752284126771,2.30081770465715));
#9406=CARTESIAN_POINT('Ctrl Pts',(-0.829622938255556,6.13165627822366,2.331603439921));
#9407=CARTESIAN_POINT('Ctrl Pts',(-0.878545941878122,6.13579788374344,2.36245001444442));
#9408=CARTESIAN_POINT('Ctrl Pts',(-0.925686956785633,6.13993948926323,2.39599138361088));
#9409=CARTESIAN_POINT('Ctrl Pts',(-0.970747883840826,6.14408109478302,2.43198145370053));
#9410=CARTESIAN_POINT('Ctrl Pts',(-1.01357450436761,6.14801734242724,2.46618698774501));
#9411=CARTESIAN_POINT('Ctrl Pts',(-1.05452218822353,6.15195359007147,2.50260381659366));
#9412=CARTESIAN_POINT('Ctrl Pts',(-1.09336663524267,6.15588983771569,2.54099054071577));
#9413=CARTESIAN_POINT('Ctrl Pts',(-1.13438238376156,6.16004611115688,2.58152298084243));
#9414=CARTESIAN_POINT('Ctrl Pts',(-1.17322572607311,6.16420238459808,2.62442275623432));
#9415=CARTESIAN_POINT('Ctrl Pts',(-1.20961240641222,6.16835865803927,2.66942817221143));
#9416=CARTESIAN_POINT('Ctrl Pts',(-1.24593408982706,6.17250750719808,2.7143531957596));
#9417=CARTESIAN_POINT('Ctrl Pts',(-1.27980749926491,6.17665635635688,2.76137599322715));
#9418=CARTESIAN_POINT('Ctrl Pts',(-1.31098563418946,6.18080520551568,2.81019860294001));
#9419=CARTESIAN_POINT('Ctrl Pts',(-1.34213255272879,6.18494990073539,2.85897233014607));
#9420=CARTESIAN_POINT('Ctrl Pts',(-1.37058926659056,6.1890945959551,2.90954186382704));
#9421=CARTESIAN_POINT('Ctrl Pts',(-1.39615050966621,6.19323929117481,2.96157816317092));
#9422=CARTESIAN_POINT('Ctrl Pts',(-1.42169588327082,6.19738141319725,3.0135821562399));
#9423=CARTESIAN_POINT('Ctrl Pts',(-1.44434912188288,6.20152353521969,3.06705064508012));
#9424=CARTESIAN_POINT('Ctrl Pts',(-1.46395068420033,6.20566565724214,3.12162964991982));
#9425=CARTESIAN_POINT('Ctrl Pts',(-1.48354753270481,6.20980678316089,3.17619552951894));
#9426=CARTESIAN_POINT('Ctrl Pts',(-1.50009398675634,6.21394790907964,3.23187090709963));
#9427=CARTESIAN_POINT('Ctrl Pts',(-1.513479294399,6.2180890349984,3.28828351686981));
#9428=CARTESIAN_POINT('Ctrl Pts',(-1.52687612511417,6.22223372590763,3.34474469082773));
#9429=CARTESIAN_POINT('Ctrl Pts',(-1.53710624944037,6.22637841681685,3.40194385993304));
#9430=CARTESIAN_POINT('Ctrl Pts',(-1.5441096675528,6.23052310772608,3.4594966647576));
#9431=CARTESIAN_POINT('Ctrl Pts',(-1.55111584629894,6.23466943240518,3.51707215596341));
#9432=CARTESIAN_POINT('Ctrl Pts',(-1.55489274683005,6.23881575708427,3.57500104238098));
#9433=CARTESIAN_POINT('Ctrl Pts',(-1.55543242157753,6.24296208176336,3.63289509224643));
#9434=CARTESIAN_POINT('Ctrl Pts',(-1.55597311345118,6.24711622102969,3.69089825515483));
#9435=CARTESIAN_POINT('Ctrl Pts',(-1.55326440933669,6.25127036029601,3.74886593033459));
#9436=CARTESIAN_POINT('Ctrl Pts',(-1.54735052601686,6.25542449956233,3.80641207622512));
#9437=CARTESIAN_POINT('Ctrl Pts',(-1.54189672524708,6.25925545913714,3.85948130295519));
#9438=CARTESIAN_POINT('Ctrl Pts',(-1.53371769744795,6.26308641871195,3.91219178420149));
#9439=CARTESIAN_POINT('Ctrl Pts',(-1.52288640708489,6.26691737828676,3.96424970512882));
#9440=CARTESIAN_POINT('Ctrl Pts',(-1.51114266458232,6.27107106646946,4.02069310181546));
#9441=CARTESIAN_POINT('Ctrl Pts',(-1.49623281783691,6.27522475465216,4.07659759798717));
#9442=CARTESIAN_POINT('Ctrl Pts',(-1.47822260570092,6.27937844283486,4.13158263211565));
#9443=CARTESIAN_POINT('Ctrl Pts',(-1.460243690403,6.28352491304002,4.1864721172469));
#9444=CARTESIAN_POINT('Ctrl Pts',(-1.43917526453003,6.28767138324519,4.24044482260319));
#9445=CARTESIAN_POINT('Ctrl Pts',(-1.41513374529266,6.29181785345036,4.29313182428395));
#9446=CARTESIAN_POINT('Ctrl Pts',(-1.39111557691066,6.29596029630497,4.34576765255325));
#9447=CARTESIAN_POINT('Ctrl Pts',(-1.36413025170531,6.30010273915958,4.39711978172299));
#9448=CARTESIAN_POINT('Ctrl Pts',(-1.33434292531336,6.30424518201418,4.44683752921203));
#9449=CARTESIAN_POINT('Ctrl Pts',(-1.30457317577932,6.30838518050274,4.49652593933218));
#9450=CARTESIAN_POINT('Ctrl Pts',(-1.2720049692522,6.31252517899129,4.54458143538888));
#9451=CARTESIAN_POINT('Ctrl Pts',(-1.23684919659392,6.31666517747985,4.59067826168063));
#9452=CARTESIAN_POINT('Ctrl Pts',(-1.20170076825582,6.32080431108983,4.63676545797918));
#9453=CARTESIAN_POINT('Ctrl Pts',(-1.1639661618001,6.32494344469982,4.68089438451617));
#9454=CARTESIAN_POINT('Ctrl Pts',(-1.12389806613617,6.3290825783098,4.72277039647614));
#9455=CARTESIAN_POINT('Ctrl Pts',(-1.08379334396079,6.33322549552921,4.76468468757582));
#9456=CARTESIAN_POINT('Ctrl Pts',(-1.04135122909556,6.33736841274863,4.80434157222005));
#9457=CARTESIAN_POINT('Ctrl Pts',(-0.996862078378742,6.34151132996804,4.84148250804075));
#9458=CARTESIAN_POINT('Ctrl Pts',(-0.952354128903536,6.34565599776481,4.87863913765347));
#9459=CARTESIAN_POINT('Ctrl Pts',(-0.905797835747481,6.34980066556158,4.91327738756306));
#9460=CARTESIAN_POINT('Ctrl Pts',(-0.857514990188483,6.35394533335835,4.94518038730212));
#9461=CARTESIAN_POINT('Ctrl Pts',(-0.809138592895801,6.35809803176834,4.97714520156145));
#9462=CARTESIAN_POINT('Ctrl Pts',(-0.759029407425855,6.36225073017833,5.0063639114422));
#9463=CARTESIAN_POINT('Ctrl Pts',(-0.707535639226758,6.36640342858832,5.03266468352131));
#9464=CARTESIAN_POINT('Ctrl Pts',(-0.659830527519038,6.37025059201149,5.05703037501979));
#9465=CARTESIAN_POINT('Ctrl Pts',(-0.610937638366417,6.37409775543467,5.07889208943651));
#9466=CARTESIAN_POINT('Ctrl Pts',(-0.561147201320725,6.37794491885785,5.09815084633289));
#9467=CARTESIAN_POINT('Ctrl Pts',(-0.508025345062969,6.38204949143226,5.11869818385905));
#9468=CARTESIAN_POINT('Ctrl Pts',(-0.453648599692884,6.38615406400668,5.13637204992538));
#9469=CARTESIAN_POINT('Ctrl Pts',(-0.398362951921492,6.3902586365811,5.15101915833668));
#9470=CARTESIAN_POINT('Ctrl Pts',(-0.342962769754882,6.39437171253309,5.16569661092899));
#9471=CARTESIAN_POINT('Ctrl Pts',(-0.286650394655885,6.39848478848509,5.17733450259257));
#9472=CARTESIAN_POINT('Ctrl Pts',(-0.22979457218428,6.40259786443708,5.18582701623475));
#9473=CARTESIAN_POINT('Ctrl Pts',(-0.173213084478156,6.40669109440536,5.19427855268872));
#9474=CARTESIAN_POINT('Ctrl Pts',(-0.116093905813107,6.41078432437364,5.19961488454923));
#9475=CARTESIAN_POINT('Ctrl Pts',(-0.0588132952565892,6.41487755434192,
5.20178220829634));
#9476=CARTESIAN_POINT('Ctrl Pts',(-0.00156603026122423,6.41896840146112,
5.20394827034903));
#9477=CARTESIAN_POINT('Ctrl Pts',(0.055841949335377,6.42305924858032,5.20294895786843));
#9478=CARTESIAN_POINT('Ctrl Pts',(0.113030086156636,6.42715009569952,5.19878237903457));
#9479=CARTESIAN_POINT('Ctrl Pts',(0.170208018481566,6.43124021285903,5.19461654367376));
#9480=CARTESIAN_POINT('Ctrl Pts',(0.22716565483362,6.43533033001855,5.18728460211642));
#9481=CARTESIAN_POINT('Ctrl Pts',(0.283525656181328,6.43942044717806,5.17683667127388));
#9482=CARTESIAN_POINT('Ctrl Pts',(0.340426053087732,6.4435497815323,5.16628856272926));
#9483=CARTESIAN_POINT('Ctrl Pts',(0.396716744592929,6.44767911588654,5.15256446132537));
#9484=CARTESIAN_POINT('Ctrl Pts',(0.452020739194503,6.45180845024077,5.13576858164988));
#9485=CARTESIAN_POINT('Ctrl Pts',(0.506884898051872,6.45590494376928,5.11910628053937));
#9486=CARTESIAN_POINT('Ctrl Pts',(0.560777515795683,6.4600014372978,5.09942113678421));
#9487=CARTESIAN_POINT('Ctrl Pts',(0.613349278357484,6.46409793082631,5.0768639197722));
#9488=CARTESIAN_POINT('Ctrl Pts',(0.666553227964308,6.46824368559341,5.05403544724826));
#9489=CARTESIAN_POINT('Ctrl Pts',(0.718403838885254,6.47238944036051,5.02826561058249));
#9490=CARTESIAN_POINT('Ctrl Pts',(0.768565993296087,6.47653519512761,4.99975779370674));
#9491=CARTESIAN_POINT('Ctrl Pts',(0.818728147706923,6.48068094989471,4.97124997683099));
#9492=CARTESIAN_POINT('Ctrl Pts',(0.867201424458467,6.48482670466182,4.94000455072265));
#9493=CARTESIAN_POINT('Ctrl Pts',(0.913684566917058,6.48897245942892,4.90626728242261));
#9494=CARTESIAN_POINT('Ctrl Pts',(0.962777192462072,6.4933509496862,4.87063606232941));
#9495=CARTESIAN_POINT('Ctrl Pts',(1.00987680836232,6.49772943994348,4.83206076559068));
#9496=CARTESIAN_POINT('Ctrl Pts',(1.05462032230712,6.50210793020077,4.79079126108015));
#9497=CARTESIAN_POINT('Ctrl Pts',(1.09777523852538,6.50633096419064,4.75098701120122));
#9498=CARTESIAN_POINT('Ctrl Pts',(1.13873813199973,6.51055399818052,4.70867701401803));
#9499=CARTESIAN_POINT('Ctrl Pts',(1.17721363608817,6.5147770321704,4.66412860512008));
#9500=CARTESIAN_POINT('Ctrl Pts',(1.21564211240262,6.51899490443744,4.61963464677593));
#9501=CARTESIAN_POINT('Ctrl Pts',(1.25158891032137,6.52321277670449,4.57290807962868));
#9502=CARTESIAN_POINT('Ctrl Pts',(1.28479547448401,6.52743064897153,4.52425297382819));
#9503=CARTESIAN_POINT('Ctrl Pts',(1.31797247820949,6.53164476649456,4.4756411807351));
#9504=CARTESIAN_POINT('Ctrl Pts',(1.34841381229424,6.53585888401758,4.42510466592981));
#9505=CARTESIAN_POINT('Ctrl Pts',(1.37590239079675,6.54007300154061,4.37297896439703));
#9506=CARTESIAN_POINT('Ctrl Pts',(1.40337562050346,6.54428476602711,4.32088236828884));
#9507=CARTESIAN_POINT('Ctrl Pts',(1.42789913910851,6.5484965305136,4.26719878661907));
#9508=CARTESIAN_POINT('Ctrl Pts',(1.44930121642437,6.5527082950001,4.21228935591415));
#9509=CARTESIAN_POINT('Ctrl Pts',(1.47070504865124,6.55692040483961,4.15737542278817));
#9510=CARTESIAN_POINT('Ctrl Pts',(1.48898673885858,6.56113251467912,4.10123589863118));
#9511=CARTESIAN_POINT('Ctrl Pts',(1.50402284555276,6.56534462451862,4.04425153330273));
#9512=CARTESIAN_POINT('Ctrl Pts',(1.51905965343888,6.56955693078514,3.9872645105724));
#9513=CARTESIAN_POINT('Ctrl Pts',(1.53085045935565,6.57376923705166,3.92943305062013));
#9514=CARTESIAN_POINT('Ctrl Pts',(1.53932242567221,6.57798154331818,3.87115040635621));
#9515=CARTESIAN_POINT('Ctrl Pts',(1.54780101708119,6.58219714361554,3.81282218496285));
#9516=CARTESIAN_POINT('Ctrl Pts',(1.55295552961869,6.58641274391291,3.75404256799067));
#9517=CARTESIAN_POINT('Ctrl Pts',(1.55476488354476,6.59062834421027,3.69521085560087));
#9518=CARTESIAN_POINT('Ctrl Pts',(1.55525530406377,6.59177097134141,3.67926467806828));
#9519=CARTESIAN_POINT('Ctrl Pts',(1.55550026292146,6.59291359847256,3.66331467869636));
#9520=CARTESIAN_POINT('Ctrl Pts',(1.55549999978821,6.5940562256037,3.64736879997355));
#9521=CARTESIAN_POINT('Ctrl Pts',(1.55415988380114,5.7559437743963,3.64862366743361));
#9522=CARTESIAN_POINT('Ctrl Pts',(1.55156969786396,5.78090458864165,3.29945639063284));
#9523=CARTESIAN_POINT('Ctrl Pts',(1.26257785748727,5.84287458307736,2.42869791902303));
#9524=CARTESIAN_POINT('Ctrl Pts',(-0.17968266065122,5.94185375770343,1.81826775193874));
#9525=CARTESIAN_POINT('Ctrl Pts',(-1.63338127522104,6.05288129827452,2.80478342088779));
#9526=CARTESIAN_POINT('Ctrl Pts',(-1.5946610617751,6.16390883884559,4.56100604319437));
#9527=CARTESIAN_POINT('Ctrl Pts',(-0.0991443931483716,6.27493637941668,
5.48278383251785));
#9528=CARTESIAN_POINT('Ctrl Pts',(1.29176384967164,6.37228135793357,4.82025828670267));
#9529=CARTESIAN_POINT('Ctrl Pts',(1.55167090461383,6.43261715626011,3.97306868873034));
#9530=CARTESIAN_POINT('Ctrl Pts',(1.55356356749417,6.4559437743963,3.64654650170336));
#9531=CARTESIAN_POINT('Origin',(0.,0.,3.64739446828387));
#9532=CARTESIAN_POINT('',(1.95399957629683,2.72586969217418,3.64868125956088));
#9533=CARTESIAN_POINT('',(1.95399895847038,2.6241303079204,3.64941196591101));
#9534=CARTESIAN_POINT('',(1.954,4.33875158023511E-16,3.64739446828387));
#9535=CARTESIAN_POINT('',(-0.861527974718931,2.50004110459941,5.40121474093917));
#9536=CARTESIAN_POINT('Ctrl Pts',(1.95399957629626,2.72586969212423,3.64868126043293));
#9537=CARTESIAN_POINT('Ctrl Pts',(1.95395422424648,2.72192515475357,3.71754854884412));
#9538=CARTESIAN_POINT('Ctrl Pts',(1.95026833624108,2.71798061738291,3.78630291233304));
#9539=CARTESIAN_POINT('Ctrl Pts',(1.94297611333583,2.71403608001225,3.85466198384382));
#9540=CARTESIAN_POINT('Ctrl Pts',(1.93571830868517,2.71011016029676,3.92269841026301));
#9541=CARTESIAN_POINT('Ctrl Pts',(1.9248684896971,2.70618424058127,3.99048552896689));
#9542=CARTESIAN_POINT('Ctrl Pts',(1.91045410367944,2.70225832086578,4.05761528410676));
#9543=CARTESIAN_POINT('Ctrl Pts',(1.8960614340148,2.69833831584263,4.12464390323853));
#9544=CARTESIAN_POINT('Ctrl Pts',(1.87811495873726,2.69441831081948,4.19101664947787));
#9545=CARTESIAN_POINT('Ctrl Pts',(1.85669380632823,2.69049830579632,4.25633133655707));
#9546=CARTESIAN_POINT('Ctrl Pts',(1.83529812509749,2.68658296192047,4.32156836011904));
#9547=CARTESIAN_POINT('Ctrl Pts',(1.81043612540151,2.68266761804462,4.38574936031787));
#9548=CARTESIAN_POINT('Ctrl Pts',(1.7822374088651,2.67875227416877,4.44848486171136));
#9549=CARTESIAN_POINT('Ctrl Pts',(1.75405663245768,2.67483942124935,4.51118045054408));
#9550=CARTESIAN_POINT('Ctrl Pts',(1.72254355119803,2.67092656832992,4.57243191939909));
#9551=CARTESIAN_POINT('Ctrl Pts',(1.68787623580038,2.6670137154105,4.63186885221691));
#9552=CARTESIAN_POINT('Ctrl Pts',(1.65321921124911,2.66310202400496,4.69128814143188));
#9553=CARTESIAN_POINT('Ctrl Pts',(1.61541005819025,2.65919033259943,4.74889354119141));
#9554=CARTESIAN_POINT('Ctrl Pts',(1.57467238540507,2.65527864119389,4.80433996338842));
#9555=CARTESIAN_POINT('Ctrl Pts',(1.5339329814046,2.65136678355451,4.85978874187353));
#9556=CARTESIAN_POINT('Ctrl Pts',(1.49026510259552,2.64745492591513,4.91307796744393));
#9557=CARTESIAN_POINT('Ctrl Pts',(1.44393413822844,2.64354306827575,4.96389369139739));
#9558=CARTESIAN_POINT('Ctrl Pts',(1.39755578074633,2.63962720909827,5.01476139603986));
#9559=CARTESIAN_POINT('Ctrl Pts',(1.34850923151036,2.6357113499208,5.06315018672279));
#9560=CARTESIAN_POINT('Ctrl Pts',(1.29709774028559,2.63179549074332,5.10878197751816));
#9561=CARTESIAN_POINT('Ctrl Pts',(1.24565650863508,2.62787736632676,5.15444016530871));
#9562=CARTESIAN_POINT('Ctrl Pts',(1.19184799458143,2.6239592419102,5.1973378728402));
#9563=CARTESIAN_POINT('Ctrl Pts',(1.13600746521101,2.62004111749364,5.23723818355429));
#9564=CARTESIAN_POINT('Ctrl Pts',(1.08007370311047,2.61611645127957,5.27720511281484));
#9565=CARTESIAN_POINT('Ctrl Pts',(1.02210156682617,2.61219178506549,5.31416439325118));
#9566=CARTESIAN_POINT('Ctrl Pts',(0.962453365994499,2.60826711885142,5.34792365600335));
#9567=CARTESIAN_POINT('Ctrl Pts',(0.935812900823456,2.606514259048,5.36300143623828));
#9568=CARTESIAN_POINT('Ctrl Pts',(0.908838399944807,2.60476139924459,5.37744152154718));
#9569=CARTESIAN_POINT('Ctrl Pts',(0.881563413985291,2.60300853944117,5.39122988113756));
#9570=CARTESIAN_POINT('Ctrl Pts',(0.821169396672914,2.59912724522269,5.4217609482863));
#9571=CARTESIAN_POINT('Ctrl Pts',(0.759058631374219,2.59524595100421,5.44921582459446));
#9572=CARTESIAN_POINT('Ctrl Pts',(0.695580341215194,2.59136465678573,5.47339665582773));
#9573=CARTESIAN_POINT('Ctrl Pts',(0.632208367608052,2.58748986314906,5.49753698781957));
#9574=CARTESIAN_POINT('Ctrl Pts',(0.567473881608393,2.58361506951239,5.51841398464903));
#9575=CARTESIAN_POINT('Ctrl Pts',(0.50174941555491,2.57974027587572,5.53587627227095));
#9576=CARTESIAN_POINT('Ctrl Pts',(0.436086388368659,2.5758691043747,5.55332223624302));
#9577=CARTESIAN_POINT('Ctrl Pts',(0.369435697939357,2.57199793287368,5.56735968916256));
#9578=CARTESIAN_POINT('Ctrl Pts',(0.302187103605554,2.56812676137267,5.5778863627021));
#9579=CARTESIAN_POINT('Ctrl Pts',(0.234977238724878,2.56425781933617,5.58840697377575));
#9580=CARTESIAN_POINT('Ctrl Pts',(0.167170647737113,2.56038887729967,5.5954207372019));
#9581=CARTESIAN_POINT('Ctrl Pts',(0.0991674998867616,2.55651993526318,5.59887641976746));
#9582=CARTESIAN_POINT('Ctrl Pts',(0.0311791136326737,2.55265183306663,5.60233135220024));
#9583=CARTESIAN_POINT('Ctrl Pts',(-0.0370052435432233,2.54878373087009,
5.60222971205842));
#9584=CARTESIAN_POINT('Ctrl Pts',(-0.10498201457924,2.54491562867354,5.59857226044298));
#9585=CARTESIAN_POINT('Ctrl Pts',(-0.173013569664411,2.54104440908413,5.59491186120284));
#9586=CARTESIAN_POINT('Ctrl Pts',(-0.240836701824025,2.53717318949472,5.58768995036119));
#9587=CARTESIAN_POINT('Ctrl Pts',(-0.308050758921072,2.53330196990531,5.5769593751808));
#9588=CARTESIAN_POINT('Ctrl Pts',(-0.37529051978522,2.52942926989751,5.56622469645098));
#9589=CARTESIAN_POINT('Ctrl Pts',(-0.441920249618324,2.5255565698897,5.55197878458949));
#9590=CARTESIAN_POINT('Ctrl Pts',(-0.507550177318502,2.5216838698819,5.5343255262465));
#9591=CARTESIAN_POINT('Ctrl Pts',(-0.573294272066751,2.51780443308885,5.51664155904149));
#9592=CARTESIAN_POINT('Ctrl Pts',(-0.638034611784078,2.51392499629581,5.49553856038446));
#9593=CARTESIAN_POINT('Ctrl Pts',(-0.701398004787334,2.51004555950277,5.47116990371455));
#9594=CARTESIAN_POINT('Ctrl Pts',(-0.755866066488291,2.50671074120165,5.45022226451539));
#9595=CARTESIAN_POINT('Ctrl Pts',(-0.8093167998603,2.50337592290053,5.42686240189678));
#9596=CARTESIAN_POINT('Ctrl Pts',(-0.861527974718931,2.50004110459941,5.40121474093917));
#9597=CARTESIAN_POINT('',(0.861525859670532,2.5,5.40121577991141));
#9598=CARTESIAN_POINT('Origin',(-5.55111512312578E-16,2.5,3.64739446828387));
#9599=CARTESIAN_POINT('Ctrl Pts',(0.861525859670531,2.5,5.40121577991141));
#9600=CARTESIAN_POINT('Ctrl Pts',(0.924640824599862,2.50400926879465,5.37021195183707));
#9601=CARTESIAN_POINT('Ctrl Pts',(0.98612780568499,2.5080185375893,5.33577388677797));
#9602=CARTESIAN_POINT('Ctrl Pts',(1.04560615745964,2.51202780638395,5.2980984888407));
#9603=CARTESIAN_POINT('Ctrl Pts',(1.10680124187082,2.51615279530842,5.25933566021137));
#9604=CARTESIAN_POINT('Ctrl Pts',(1.16586949339281,2.52027778423288,5.21714593155204));
#9605=CARTESIAN_POINT('Ctrl Pts',(1.22242491847299,2.52440277315734,5.1717937987404));
#9606=CARTESIAN_POINT('Ctrl Pts',(1.27735367946414,2.52840911791387,5.12774609756729));
#9607=CARTESIAN_POINT('Ctrl Pts',(1.3299118591709,2.53241546267039,5.08071578688038));
#9608=CARTESIAN_POINT('Ctrl Pts',(1.37977792362144,2.53642180742692,5.03098721236969));
#9609=CARTESIAN_POINT('Ctrl Pts',(1.42964495246872,2.54042822966511,4.98125767612126));
#9610=CARTESIAN_POINT('Ctrl Pts',(1.47681943741636,2.5444346519033,4.92883009647145));
#9611=CARTESIAN_POINT('Ctrl Pts',(1.52101670404325,2.5484410741415,4.87402570301639));
#9612=CARTESIAN_POINT('Ctrl Pts',(1.56522679197008,2.55244865861313,4.81920541121239));
#9613=CARTESIAN_POINT('Ctrl Pts',(1.60645765682533,2.55645624308476,4.76200729257364));
#9614=CARTESIAN_POINT('Ctrl Pts',(1.6444657981191,2.5604638275564,4.7027845567424));
#9615=CARTESIAN_POINT('Ctrl Pts',(1.68442820694257,2.56467747030762,4.64051676093939));
#9616=CARTESIAN_POINT('Ctrl Pts',(1.72082726588756,2.56889111305884,4.57601102517069));
#9617=CARTESIAN_POINT('Ctrl Pts',(1.75343383018526,2.57310475581007,4.5097086819913));
#9618=CARTESIAN_POINT('Ctrl Pts',(1.78451254633702,2.57712095959758,4.44651307251045));
#9619=CARTESIAN_POINT('Ctrl Pts',(1.81214608686432,2.5811371633851,4.3816859091714));
#9620=CARTESIAN_POINT('Ctrl Pts',(1.83618572392648,2.58515336717261,4.3156294473508));
#9621=CARTESIAN_POINT('Ctrl Pts',(1.86024744854126,2.58917326103715,4.24951229303422));
#9622=CARTESIAN_POINT('Ctrl Pts',(1.88070855939279,2.59319315490169,4.18216402918135));
#9623=CARTESIAN_POINT('Ctrl Pts',(1.89747052412524,2.59721304876623,4.11400095138918));
#9624=CARTESIAN_POINT('Ctrl Pts',(1.91426290407195,2.6012402368791,4.04571418913342));
#9625=CARTESIAN_POINT('Ctrl Pts',(1.92734265511498,2.60526742499197,3.97661011190263));
#9626=CARTESIAN_POINT('Ctrl Pts',(1.93666260885463,2.60929461310484,3.90711343074976));
#9627=CARTESIAN_POINT('Ctrl Pts',(1.93799942281075,2.60987225559359,3.89714512662895));
#9628=CARTESIAN_POINT('Ctrl Pts',(1.93925897094148,2.61044989808234,3.88716874862352));
#9629=CARTESIAN_POINT('Ctrl Pts',(1.94044120187923,2.61102754057108,3.87718555176946));
#9630=CARTESIAN_POINT('Ctrl Pts',(1.94938012008528,2.61539512967265,3.80170200852605));
#9631=CARTESIAN_POINT('Ctrl Pts',(1.95392024650498,2.61976271877421,3.72564652348674));
#9632=CARTESIAN_POINT('Ctrl Pts',(1.95399895846957,2.62413030787577,3.64941196669006));
#9633=CARTESIAN_POINT('Origin',(0.,0.,3.64739446828387));
#9634=CARTESIAN_POINT('',(1.95399979033444,3.42586969208078,3.64829966051471));
#9635=CARTESIAN_POINT('',(1.95399983251307,3.3241303078362,3.64820350405597));
#9636=CARTESIAN_POINT('',(1.954,4.33875158023511E-16,3.64739446828387));
#9637=CARTESIAN_POINT('Ctrl Pts',(1.95399979033444,3.42586969208078,3.64829966051471));
#9638=CARTESIAN_POINT('Ctrl Pts',(1.95396480342058,3.42158392528816,3.72382441647484));
#9639=CARTESIAN_POINT('Ctrl Pts',(1.94954693631289,3.41729815849555,3.79920428739692));
#9640=CARTESIAN_POINT('Ctrl Pts',(1.94082130003993,3.41301239170294,3.87395280803618));
#9641=CARTESIAN_POINT('Ctrl Pts',(1.93206695591947,3.40871252448995,3.94894725562724));
#9642=CARTESIAN_POINT('Ctrl Pts',(1.91897658649658,3.40441265727697,4.0233058867645));
#9643=CARTESIAN_POINT('Ctrl Pts',(1.90167612158761,3.40011279006398,4.09655360331678));
#9644=CARTESIAN_POINT('Ctrl Pts',(1.88429615383603,3.39579316317008,4.17013792363729));
#9645=CARTESIAN_POINT('Ctrl Pts',(1.86266745413099,3.39147353627618,4.24260079990362));
#9646=CARTESIAN_POINT('Ctrl Pts',(1.83696603276115,3.38715390938228,4.31348139540507));
#9647=CARTESIAN_POINT('Ctrl Pts',(1.8231769297256,3.38483638073443,4.35150963596523));
#9648=CARTESIAN_POINT('Ctrl Pts',(1.80821632797973,3.38251885208658,4.38908280851349));
#9649=CARTESIAN_POINT('Ctrl Pts',(1.79211686507899,3.38020132343873,4.4261326411632));
#9650=CARTESIAN_POINT('Ctrl Pts',(1.76489513180678,3.37628273639694,4.48877825042292));
#9651=CARTESIAN_POINT('Ctrl Pts',(1.73433083910883,3.37236414935515,4.55011866002973));
#9652=CARTESIAN_POINT('Ctrl Pts',(1.70057119742648,3.36844556231337,4.60977360484257));
#9653=CARTESIAN_POINT('Ctrl Pts',(1.66686231904713,3.36453286752669,4.66933884840599));
#9654=CARTESIAN_POINT('Ctrl Pts',(1.62996786774875,3.36062017274002,4.72722323253675));
#9655=CARTESIAN_POINT('Ctrl Pts',(1.59008264753988,3.35670747795335,4.7830674731548));
#9656=CARTESIAN_POINT('Ctrl Pts',(1.55024424507099,3.35279937593377,4.83884616314725));
#9657=CARTESIAN_POINT('Ctrl Pts',(1.50742233031503,3.3488912739142,4.89258906739672));
#9658=CARTESIAN_POINT('Ctrl Pts',(1.46185610518547,3.34498317189463,4.94396406831773));
#9659=CARTESIAN_POINT('Ctrl Pts',(1.4163183760412,3.34107751390498,4.99530694058937));
#9660=CARTESIAN_POINT('Ctrl Pts',(1.36804006657401,3.33717185591533,5.044284479995));
#9661=CARTESIAN_POINT('Ctrl Pts',(1.31730095029969,3.33326619792568,5.09059722823811));
#9662=CARTESIAN_POINT('Ctrl Pts',(1.26657617424462,3.3293616437785,5.13689688727091));
#9663=CARTESIAN_POINT('Ctrl Pts',(1.21339233509797,3.32545708963133,5.18053291892599));
#9664=CARTESIAN_POINT('Ctrl Pts',(1.15806508986361,3.32155253548416,5.22124365027025));
#9665=CARTESIAN_POINT('Ctrl Pts',(1.10273451884996,3.3176477466301,5.26195682877967));
#9666=CARTESIAN_POINT('Ctrl Pts',(1.04526068354755,3.31374295777605,5.29974406850755));
#9667=CARTESIAN_POINT('Ctrl Pts',(0.985989779129751,3.30983816892199,5.33438591919631));
#9668=CARTESIAN_POINT('Ctrl Pts',(0.926655846197206,3.30592922772634,5.36906460793265));
#9669=CARTESIAN_POINT('Ctrl Pts',(0.865521455784724,3.30202028653069,5.40059098391652));
#9670=CARTESIAN_POINT('Ctrl Pts',(0.802958182434712,3.29811134533503,5.42879115551026));
#9671=CARTESIAN_POINT('Ctrl Pts',(0.740357429382511,3.29420006241485,5.45700822094564));
#9672=CARTESIAN_POINT('Ctrl Pts',(0.676326548180425,3.29028877949467,5.4818949381124));
#9673=CARTESIAN_POINT('Ctrl Pts',(0.61125527900254,3.28637749657449,5.50332630536505));
#9674=CARTESIAN_POINT('Ctrl Pts',(0.546072049952875,3.28245948400634,5.52479454685053));
#9675=CARTESIAN_POINT('Ctrl Pts',(0.479845334551204,3.27854147143819,5.54279544405977));
#9676=CARTESIAN_POINT('Ctrl Pts',(0.412977281260173,3.27462345887005,5.55725461111186));
#9677=CARTESIAN_POINT('Ctrl Pts',(0.381974383829435,3.27280690020258,5.56395850110099));
#9678=CARTESIAN_POINT('Ctrl Pts',(0.350833722259817,3.27099034153511,5.56990177297914));
#9679=CARTESIAN_POINT('Ctrl Pts',(0.319595685371466,3.26917378286764,5.57508080114302));
#9680=CARTESIAN_POINT('Ctrl Pts',(0.252208833978639,3.2652550933095,5.58625302692934));
#9681=CARTESIAN_POINT('Ctrl Pts',(0.184102294733262,3.26133640375136,5.59390957506826));
#9682=CARTESIAN_POINT('Ctrl Pts',(0.115675333849662,3.25741771419322,5.59796751668241));
#9683=CARTESIAN_POINT('Ctrl Pts',(0.047351216489819,3.25350491429959,5.60201935934068));
#9684=CARTESIAN_POINT('Ctrl Pts',(-0.0212918798043706,3.24959211440596,
5.60248330086764));
#9685=CARTESIAN_POINT('Ctrl Pts',(-0.0898464570696235,3.24567931451232,
5.59932776994969));
#9686=CARTESIAN_POINT('Ctrl Pts',(-0.158320623613156,3.24177110411623,5.59617594029471));
#9687=CARTESIAN_POINT('Ctrl Pts',(-0.226705988457172,3.23786289372013,5.58941309229315));
#9688=CARTESIAN_POINT('Ctrl Pts',(-0.294593750439108,3.23395468332403,5.57905968829541));
#9689=CARTESIAN_POINT('Ctrl Pts',(-0.362439092315836,3.23004891499837,5.56871275368882));
#9690=CARTESIAN_POINT('Ctrl Pts',(-0.429786963122477,3.2261431466727,5.55477978767468));
#9691=CARTESIAN_POINT('Ctrl Pts',(-0.496233948595555,3.22223737834703,5.53733305677326));
#9692=CARTESIAN_POINT('Ctrl Pts',(-0.562662185118731,3.21833271208874,5.51989124871193));
#9693=CARTESIAN_POINT('Ctrl Pts',(-0.628189565578085,3.21442804583045,5.49893776883437));
#9694=CARTESIAN_POINT('Ctrl Pts',(-0.692424912524393,3.21052337957215,5.4745955356313));
#9695=CARTESIAN_POINT('Ctrl Pts',(-0.756664146815767,3.20661847701428,5.45025182930378));
#9696=CARTESIAN_POINT('Ctrl Pts',(-0.819610733474382,3.20271357445642,5.42251913914845));
#9697=CARTESIAN_POINT('Ctrl Pts',(-0.880892360436774,3.19880867189855,5.39156895764098));
#9698=CARTESIAN_POINT('Ctrl Pts',(-0.942239177187545,3.1948996154077,5.36058585214172));
#9699=CARTESIAN_POINT('Ctrl Pts',(-1.00191705989154,3.19099055891685,5.32637864684416));
#9700=CARTESIAN_POINT('Ctrl Pts',(-1.05957816435751,3.187081502426,5.28916488878023));
#9701=CARTESIAN_POINT('Ctrl Pts',(-1.11727382662157,3.18317010313603,5.25192882754417));
#9702=CARTESIAN_POINT('Ctrl Pts',(-1.17294990653501,3.17925870384606,5.21168291548391));
#9703=CARTESIAN_POINT('Ctrl Pts',(-1.22628974279194,3.17534730455608,5.16868650688898));
#9704=CARTESIAN_POINT('Ctrl Pts',(-1.2797213569444,3.17142917521179,5.12561611756646));
#9705=CARTESIAN_POINT('Ctrl Pts',(-1.33080833887659,3.1675110458675,5.07978611454225));
#9706=CARTESIAN_POINT('Ctrl Pts',(-1.37926978606367,3.16359291652321,5.03149376286208));
#9707=CARTESIAN_POINT('Ctrl Pts',(-1.40172554595874,3.16177735844766,5.00911635737701));
#9708=CARTESIAN_POINT('Ctrl Pts',(-1.42361812047924,3.15996180037211,4.9862107284678));
#9709=CARTESIAN_POINT('Ctrl Pts',(-1.44492256927573,3.15814624229656,4.96280876378078));
#9710=CARTESIAN_POINT('Ctrl Pts',(-1.49089463538647,3.15422851803745,4.91231054728196));
#9711=CARTESIAN_POINT('Ctrl Pts',(-1.53430736323659,3.15031079377834,4.85929933663351));
#9712=CARTESIAN_POINT('Ctrl Pts',(-1.57487428716369,3.14639306951922,4.8040651126899));
#9713=CARTESIAN_POINT('Ctrl Pts',(-1.61538019121469,3.14248123821491,4.74891397085298));
#9714=CARTESIAN_POINT('Ctrl Pts',(-1.65304849789035,3.13856940691059,4.69154684530576));
#9715=CARTESIAN_POINT('Ctrl Pts',(-1.68763137962661,3.13465757560628,4.63228853695298));
#9716=CARTESIAN_POINT('Ctrl Pts',(-1.72217368614137,3.13075033395481,4.57309975487638));
#9717=CARTESIAN_POINT('Ctrl Pts',(-1.7536375103363,3.12684309230334,4.51202461959079));
#9718=CARTESIAN_POINT('Ctrl Pts',(-1.78181799743233,3.12293585065187,4.44941730089292));
#9719=CARTESIAN_POINT('Ctrl Pts',(-1.80998087476159,3.11903105060526,4.38684910502059));
#9720=CARTESIAN_POINT('Ctrl Pts',(-1.83486428347826,3.11512625055865,4.3227510726286));
#9721=CARTESIAN_POINT('Ctrl Pts',(-1.85630978619131,3.11122145051204,4.25750099807222));
#9722=CARTESIAN_POINT('Ctrl Pts',(-1.87774924678108,3.10731775061605,4.19226930727673));
#9723=CARTESIAN_POINT('Ctrl Pts',(-1.89575257068176,3.10341405072007,4.12588668583091));
#9724=CARTESIAN_POINT('Ctrl Pts',(-1.91021049363009,3.09951035082408,4.05874817256463));
#9725=CARTESIAN_POINT('Ctrl Pts',(-1.92466930422709,3.09560641125923,3.99160553730842));
#9726=CARTESIAN_POINT('Ctrl Pts',(-1.93558218067504,3.09170247169437,3.92370739958933));
#9727=CARTESIAN_POINT('Ctrl Pts',(-1.94289088911684,3.08779853212952,3.85545934515347));
#9728=CARTESIAN_POINT('Ctrl Pts',(-1.95020739604261,3.08389042701197,3.78713846918391));
#9729=CARTESIAN_POINT('Ctrl Pts',(-1.95391200778782,3.07998232189443,3.7184674215022));
#9730=CARTESIAN_POINT('Ctrl Pts',(-1.95399844922611,3.07607421677689,3.64985626071562));
#9731=CARTESIAN_POINT('Ctrl Pts',(-1.95408494259971,3.07216376361086,3.58120387730902));
#9732=CARTESIAN_POINT('Ctrl Pts',(-1.95054896473042,3.06825331044483,3.51261194378149));
#9733=CARTESIAN_POINT('Ctrl Pts',(-1.9434362803453,3.0643428572788,3.44448704053018));
#9734=CARTESIAN_POINT('Ctrl Pts',(-1.93631132208703,3.0604256561111,3.37624457879103));
#9735=CARTESIAN_POINT('Ctrl Pts',(-1.92559741588042,3.0565084549434,3.30847124143881));
#9736=CARTESIAN_POINT('Ctrl Pts',(-1.9113915795902,3.0525912537757,3.24156417188934));
#9737=CARTESIAN_POINT('Ctrl Pts',(-1.90477612677183,3.05076706975896,3.21040651578392));
#9738=CARTESIAN_POINT('Ctrl Pts',(-1.8974041141819,3.04894288574222,3.17943651304367));
#9739=CARTESIAN_POINT('Ctrl Pts',(-1.88928897332868,3.04711870172548,3.1486929791557));
#9740=CARTESIAN_POINT('Ctrl Pts',(-1.87185313432429,3.04319933921465,3.08263875816404));
#9741=CARTESIAN_POINT('Ctrl Pts',(-1.85091457533122,3.03927997670381,3.01736962809995));
#9742=CARTESIAN_POINT('Ctrl Pts',(-1.82656137564055,3.03536061419298,2.95328385676861));
#9743=CARTESIAN_POINT('Ctrl Pts',(-1.8022448089673,3.03144714733762,2.88929448571347));
#9744=CARTESIAN_POINT('Ctrl Pts',(-1.77452396902811,3.02753368048226,2.82648539634389));
#9745=CARTESIAN_POINT('Ctrl Pts',(-1.74353715277275,3.0236202136269,2.76524130873553));
#9746=CARTESIAN_POINT('Ctrl Pts',(-1.71258677063199,3.01971134820263,2.70406923156182));
#9747=CARTESIAN_POINT('Ctrl Pts',(-1.67837825975926,3.01580248277837,2.64445893807871));
#9748=CARTESIAN_POINT('Ctrl Pts',(-1.64109791096865,3.0118936173541,2.58677500466163));
#9749=CARTESIAN_POINT('Ctrl Pts',(-1.60384092725405,3.00798720177113,2.52912722405782));
#9750=CARTESIAN_POINT('Ctrl Pts',(-1.56351619100123,3.00408078618815,2.47340382040299));
#9751=CARTESIAN_POINT('Ctrl Pts',(-1.5203550367178,3.00017437060518,2.41994322186843));
#9752=CARTESIAN_POINT('Ctrl Pts',(-1.47720615483415,2.99626906576854,2.3664978242674));
#9753=CARTESIAN_POINT('Ctrl Pts',(-1.43122276464043,2.99236376093189,2.315314336752));
#9754=CARTESIAN_POINT('Ctrl Pts',(-1.38267738706858,2.98845845609525,2.26669926539179));
#9755=CARTESIAN_POINT('Ctrl Pts',(-1.33412919142794,2.98455292455488,2.21808137191705));
#9756=CARTESIAN_POINT('Ctrl Pts',(-1.28301906227187,2.98064739301452,2.17203253660852));
#9757=CARTESIAN_POINT('Ctrl Pts',(-1.22965609646498,2.97674186147416,2.12882215047135));
#9758=CARTESIAN_POINT('Ctrl Pts',(-1.17623662792966,2.97283219460914,2.08556601154146));
#9759=CARTESIAN_POINT('Ctrl Pts',(-1.12055994499601,2.96892252774412,2.04515462963031));
#9760=CARTESIAN_POINT('Ctrl Pts',(-1.06296712617754,2.96501286087911,2.00781620279428));
#9761=CARTESIAN_POINT('Ctrl Pts',(-1.00533993935781,2.96110086095524,1.97045549458486));
#9762=CARTESIAN_POINT('Ctrl Pts',(-0.945794766954578,2.95718886103137,1.93617163639363));
#9763=CARTESIAN_POINT('Ctrl Pts',(-0.884698047574256,2.9532768611075,1.90514725143481));
#9764=CARTESIAN_POINT('Ctrl Pts',(-0.823496549589744,2.94935815224908,1.87406966080824));
#9765=CARTESIAN_POINT('Ctrl Pts',(-0.760738643192554,2.94543944339066,1.84626289884297));
#9766=CARTESIAN_POINT('Ctrl Pts',(-0.696810697122993,2.94152073453224,1.82186143588622));
#9767=CARTESIAN_POINT('Ctrl Pts',(-0.667285540868792,2.93971087673963,1.81059160710359));
#9768=CARTESIAN_POINT('Ctrl Pts',(-0.637511017076782,2.93790101894702,1.80004744746111));
#9769=CARTESIAN_POINT('Ctrl Pts',(-0.607526056778454,2.93609116115441,1.79023855389886));
#9770=CARTESIAN_POINT('Ctrl Pts',(-0.54258923585884,2.93217164916575,1.76899595900015));
#9771=CARTESIAN_POINT('Ctrl Pts',(-0.476409137968989,2.9282521371771,1.75112150272362));
#9772=CARTESIAN_POINT('Ctrl Pts',(-0.409368097857574,2.92433262518844,1.73675746444026));
#9773=CARTESIAN_POINT('Ctrl Pts',(-0.342427594251089,2.92041899100293,1.72241496684607));
#9774=CARTESIAN_POINT('Ctrl Pts',(-0.274629187590647,2.91650535681741,1.71157254128802));
#9775=CARTESIAN_POINT('Ctrl Pts',(-0.206371096701374,2.9125917226319,1.70432293834827));
#9776=CARTESIAN_POINT('Ctrl Pts',(-0.138192820382465,2.9086826646809,1.6970818124101));
#9777=CARTESIAN_POINT('Ctrl Pts',(-0.0695564137906668,2.90477360672989,
1.69342521710811));
#9778=CARTESIAN_POINT('Ctrl Pts',(-0.000869236631244366,2.90086454877889,
1.69339466162378));
#9779=CARTESIAN_POINT('Ctrl Pts',(0.0677751655907483,2.8969579251936,1.69336412516787));
#9780=CARTESIAN_POINT('Ctrl Pts',(0.136469785285936,2.89305130160832,1.69695514921585));
#9781=CARTESIAN_POINT('Ctrl Pts',(0.204804767933492,2.88914467802303,1.70415721899296));
#9782=CARTESIAN_POINT('Ctrl Pts',(0.273120583999533,2.8852391501667,1.71135726873506));
#9783=CARTESIAN_POINT('Ctrl Pts',(0.341076474743505,2.88133362231037,1.72216630200453));
#9784=CARTESIAN_POINT('Ctrl Pts',(0.408267032846791,2.87742809445405,1.73652188490986));
#9785=CARTESIAN_POINT('Ctrl Pts',(0.475461741904409,2.87352232531876,1.75087835468636));
#9786=CARTESIAN_POINT('Ctrl Pts',(0.541890544378558,2.86961655618348,1.76878170389678));
#9787=CARTESIAN_POINT('Ctrl Pts',(0.607159343224885,2.86571078704819,1.7901186320294));
#9788=CARTESIAN_POINT('Ctrl Pts',(0.672497582257442,2.86180086252257,1.81147826075234));
#9789=CARTESIAN_POINT('Ctrl Pts',(0.736672886707037,2.85789093799695,1.8362786056171));
#9790=CARTESIAN_POINT('Ctrl Pts',(0.799308385936824,2.85398101347132,1.86435714277129));
#9791=CARTESIAN_POINT('Ctrl Pts',(0.861981449243666,2.85006874406607,1.89245251932719));
#9792=CARTESIAN_POINT('Ctrl Pts',(0.923112432150434,2.84615647466082,1.9238297765482));
#9793=CARTESIAN_POINT('Ctrl Pts',(0.982348966787811,2.84224420525557,1.95828034915192));
#9794=CARTESIAN_POINT('Ctrl Pts',(1.04168731167449,2.83832521180534,1.99279013219741));
#9795=CARTESIAN_POINT('Ctrl Pts',(1.09912429892471,2.8344062183551,2.03038350381037));
#9796=CARTESIAN_POINT('Ctrl Pts',(1.15433717467102,2.83048722490487,2.07080901637442));
#9797=CARTESIAN_POINT('Ctrl Pts',(1.17980738747821,2.82867935679769,2.08945768109127));
#9798=CARTESIAN_POINT('Ctrl Pts',(1.20480477019518,2.82687148869051,2.10870848800464));
#9799=CARTESIAN_POINT('Ctrl Pts',(1.229300222574,2.82506362058333,2.12853405245248));
#9800=CARTESIAN_POINT('Ctrl Pts',(1.28164323011488,2.82120048498969,2.17089822900847));
#9801=CARTESIAN_POINT('Ctrl Pts',(1.33191182350579,2.81733734939605,2.21606720796799));
#9802=CARTESIAN_POINT('Ctrl Pts',(1.37978360123067,2.81347421380241,2.26380738617631));
#9803=CARTESIAN_POINT('Ctrl Pts',(1.42757306397375,2.80961772082684,2.31146547568672));
#9804=CARTESIAN_POINT('Ctrl Pts',(1.47297353608627,2.80576122785128,2.3616856339295));
#9805=CARTESIAN_POINT('Ctrl Pts',(1.51569521873076,2.80190473487571,2.4141937531054));
#9806=CARTESIAN_POINT('Ctrl Pts',(1.55837600201868,2.79805193389146,2.46665160393613));
#9807=CARTESIAN_POINT('Ctrl Pts',(1.59838275892303,2.79419913290722,2.52139268472609));
#9808=CARTESIAN_POINT('Ctrl Pts',(1.63546324370269,2.79034633192297,2.57810686501827));
#9809=CARTESIAN_POINT('Ctrl Pts',(1.67252178951752,2.78649581047918,2.63478748991296));
#9810=CARTESIAN_POINT('Ctrl Pts',(1.7066572187371,2.78264528903539,2.69343847657475));
#9811=CARTESIAN_POINT('Ctrl Pts',(1.73765945873494,2.7787947675916,2.7537191326787));
#9812=CARTESIAN_POINT('Ctrl Pts',(1.76865469033083,2.7749451166011,2.81398616166839));
#9813=CARTESIAN_POINT('Ctrl Pts',(1.79651790755941,2.7710954656106,2.87588167785104));
#9814=CARTESIAN_POINT('Ctrl Pts',(1.82108501638625,2.76724581462011,2.93904048679333));
#9815=CARTESIAN_POINT('Ctrl Pts',(1.84567006914102,2.76339335182703,3.00224542721672));
#9816=CARTESIAN_POINT('Ctrl Pts',(1.86695402027122,2.75954088903396,3.06671503024622));
#9817=CARTESIAN_POINT('Ctrl Pts',(1.88482147805864,2.75568842624088,3.13206545119979));
#9818=CARTESIAN_POINT('Ctrl Pts',(1.90269589233817,2.7518344635351,3.19744131559885));
#9819=CARTESIAN_POINT('Ctrl Pts',(1.91715105613523,2.74798050082931,3.26369818508322));
#9820=CARTESIAN_POINT('Ctrl Pts',(1.9281225718929,2.74412653812353,3.33044124183381));
#9821=CARTESIAN_POINT('Ctrl Pts',(1.93911105040701,2.74026661691281,3.39728748817467));
#9822=CARTESIAN_POINT('Ctrl Pts',(1.94660507416332,2.7364066957021,3.46462091816702));
#9823=CARTESIAN_POINT('Ctrl Pts',(1.95059216252502,2.73254677449139,3.53204189789213));
#9824=CARTESIAN_POINT('Ctrl Pts',(1.95289118330323,2.73032108038565,3.5709179445743));
#9825=CARTESIAN_POINT('Ctrl Pts',(1.95402516604589,2.72809538627992,3.60982308596676));
#9826=CARTESIAN_POINT('Ctrl Pts',(1.95399957629683,2.72586969217418,3.64868125956088));
#9827=CARTESIAN_POINT('Ctrl Pts',(1.95399895847038,2.6241303079204,3.64941196591101));
#9828=CARTESIAN_POINT('Ctrl Pts',(1.9540679267512,2.62795723854692,3.58261439099596));
#9829=CARTESIAN_POINT('Ctrl Pts',(1.95070752961312,2.63178416917345,3.51565940348065));
#9830=CARTESIAN_POINT('Ctrl Pts',(1.94389595297049,2.63561109979997,3.4489391231179));
#9831=CARTESIAN_POINT('Ctrl Pts',(1.93709490011831,2.6394321178723,3.38232192465326));
#9832=CARTESIAN_POINT('Ctrl Pts',(1.92685329612979,2.64325313594464,3.31593922231414));
#9833=CARTESIAN_POINT('Ctrl Pts',(1.91320133873364,2.64707415401697,3.25018339408302));
#9834=CARTESIAN_POINT('Ctrl Pts',(1.89956094128294,2.65089193660013,3.18448324532446));
#9835=CARTESIAN_POINT('Ctrl Pts',(1.88251601273264,2.65470971918328,3.11940942193869));
#9836=CARTESIAN_POINT('Ctrl Pts',(1.86214838250636,2.65852750176643,3.05534767830107));
#9837=CARTESIAN_POINT('Ctrl Pts',(1.84179033870873,2.66234348743458,2.99131608659214));
#9838=CARTESIAN_POINT('Ctrl Pts',(1.81811284795109,2.66615947310273,2.92829612128937));
#9839=CARTESIAN_POINT('Ctrl Pts',(1.79124798235703,2.66997545877088,2.86665977217906));
#9840=CARTESIAN_POINT('Ctrl Pts',(1.76438566184423,2.6737910829262,2.80502926227596));
#9841=CARTESIAN_POINT('Ctrl Pts',(1.73433677346291,2.67760670708152,2.74478258014629));
#9842=CARTESIAN_POINT('Ctrl Pts',(1.70128123276098,2.68142233123684,2.68627108023461));
#9843=CARTESIAN_POINT('Ctrl Pts',(1.6681942594413,2.68524158368119,2.62770394155341));
#9844=CARTESIAN_POINT('Ctrl Pts',(1.63209518231189,2.68906083612553,2.57087572753031));
#9845=CARTESIAN_POINT('Ctrl Pts',(1.59320886633498,2.69288008856988,2.51611134358359));
#9846=CARTESIAN_POINT('Ctrl Pts',(1.55430239227122,2.69670132085779,2.46131857059618));
#9847=CARTESIAN_POINT('Ctrl Pts',(1.51260612827238,2.7005225531457,2.40859215759322));
#9848=CARTESIAN_POINT('Ctrl Pts',(1.4683851679231,2.7043437854336,2.35822380517388));
#9849=CARTESIAN_POINT('Ctrl Pts',(1.42408702466098,2.70817168726999,2.30776754023242));
#9850=CARTESIAN_POINT('Ctrl Pts',(1.37725575526897,2.71199958910637,2.25967791329002));
#9851=CARTESIAN_POINT('Ctrl Pts',(1.32819236692964,2.71582749094275,2.21420884303157));
#9852=CARTESIAN_POINT('Ctrl Pts',(1.30158539097332,2.71790335434255,2.18955105847833));
#9853=CARTESIAN_POINT('Ctrl Pts',(1.27432254066745,2.71997921774235,2.16566323416876));
#9854=CARTESIAN_POINT('Ctrl Pts',(1.24645540150732,2.72205508114215,2.14258054887282));
#9855=CARTESIAN_POINT('Ctrl Pts',(1.1937797887706,2.72597896352972,2.09894870763555));
#9856=CARTESIAN_POINT('Ctrl Pts',(1.13870787370658,2.72990284591728,2.05800107044378));
#9857=CARTESIAN_POINT('Ctrl Pts',(1.08154398218446,2.73382672830484,2.02001048943912));
#9858=CARTESIAN_POINT('Ctrl Pts',(1.02446590816368,2.73774471994961,1.98207694193321));
#9859=CARTESIAN_POINT('Ctrl Pts',(0.965302496310353,2.74166271159438,1.94709190850394));
#9860=CARTESIAN_POINT('Ctrl Pts',(0.904390978508841,2.74558070323915,1.91528795943639));
#9861=CARTESIAN_POINT('Ctrl Pts',(0.843551259159137,2.74949407661557,1.88352149875176));
#9862=CARTESIAN_POINT('Ctrl Pts',(0.780967959127656,2.753407449992,1.85492890052287));
#9863=CARTESIAN_POINT('Ctrl Pts',(0.717005575465429,2.75732082336843,1.82969839777277));
#9864=CARTESIAN_POINT('Ctrl Pts',(0.653083455404389,2.76123173332033,1.80448377734041));
#9865=CARTESIAN_POINT('Ctrl Pts',(0.587784428964954,2.76514264327222,1.78262723308196));
#9866=CARTESIAN_POINT('Ctrl Pts',(0.521494381419933,2.76905355322412,1.76426950956567));
#9867=CARTESIAN_POINT('Ctrl Pts',(0.455223518419318,2.7729633313466,1.74591709883123));
#9868=CARTESIAN_POINT('Ctrl Pts',(0.387962675909299,2.77687310946909,1.73106162924773));
#9869=CARTESIAN_POINT('Ctrl Pts',(0.32011264658097,2.78078288759157,1.71979391487584));
#9870=CARTESIAN_POINT('Ctrl Pts',(0.252259179413601,2.78469286381549,1.70852562958912));
#9871=CARTESIAN_POINT('Ctrl Pts',(0.183816950128407,2.7886028400394,1.70084553823989));
#9872=CARTESIAN_POINT('Ctrl Pts',(0.115194905210794,2.79251281626332,1.69679298827483));
#9873=CARTESIAN_POINT('Ctrl Pts',(0.0465016013761671,2.79642685270828,1.69273623003643));
#9874=CARTESIAN_POINT('Ctrl Pts',(-0.0223714004930565,2.80034088915324,
1.69231455996694));
#9875=CARTESIAN_POINT('Ctrl Pts',(-0.091013102577,2.80425492559821,1.69551521608631));
#9876=CARTESIAN_POINT('Ctrl Pts',(-0.15969507348771,2.80817125822248,1.69871774987863));
#9877=CARTESIAN_POINT('Ctrl Pts',(-0.228144986629474,2.81208759084674,1.7055467912717));
#9878=CARTESIAN_POINT('Ctrl Pts',(-0.295957695995734,2.81600392347101,1.71593775321597));
#9879=CARTESIAN_POINT('Ctrl Pts',(-0.36388478966922,2.81992686203977,1.72634624230219));
#9880=CARTESIAN_POINT('Ctrl Pts',(-0.431172054604574,2.82384980060853,1.74032854398264));
#9881=CARTESIAN_POINT('Ctrl Pts',(-0.497426112609263,2.82777273917729,1.7577693037355));
#9882=CARTESIAN_POINT('Ctrl Pts',(-0.527318777624549,2.8295427000226,1.7656382676089));
#9883=CARTESIAN_POINT('Ctrl Pts',(-0.557001347279252,2.83131266086792,1.77421058611087));
#9884=CARTESIAN_POINT('Ctrl Pts',(-0.586438997343526,2.83308262171323,1.78347244674039));
#9885=CARTESIAN_POINT('Ctrl Pts',(-0.651721774515719,2.83700779777912,1.80401212916603));
#9886=CARTESIAN_POINT('Ctrl Pts',(-0.716048236771028,2.840932973845,1.82802469709651));
#9887=CARTESIAN_POINT('Ctrl Pts',(-0.779023915909538,2.84485814991089,1.85540179574278));
#9888=CARTESIAN_POINT('Ctrl Pts',(-0.841907393739568,2.84877757921272,1.88273881218029));
#9889=CARTESIAN_POINT('Ctrl Pts',(-0.903443568159146,2.85269700851455,1.91343038786888));
#9890=CARTESIAN_POINT('Ctrl Pts',(-0.963254062177318,2.85661643781638,1.94731870182554));
#9891=CARTESIAN_POINT('Ctrl Pts',(-1.02299724079491,2.8605314558864,1.98116887522732));
#9892=CARTESIAN_POINT('Ctrl Pts',(-1.08101817229141,2.86444647395642,2.01820840058983));
#9893=CARTESIAN_POINT('Ctrl Pts',(-1.13696100915546,2.86836149202645,2.05823253076454));
#9894=CARTESIAN_POINT('Ctrl Pts',(-1.19287047242155,2.87227417452955,2.09823278390147));
#9895=CARTESIAN_POINT('Ctrl Pts',(-1.24670390311217,2.87618685703266,2.1412138249301));
#9896=CARTESIAN_POINT('Ctrl Pts',(-1.29813382908812,2.88009953953577,2.1869272273719));
#9897=CARTESIAN_POINT('Ctrl Pts',(-1.34955052697988,2.88401121567356,2.23262887205352));
#9898=CARTESIAN_POINT('Ctrl Pts',(-1.39856458168765,2.88792289181135,2.28106115747686));
#9899=CARTESIAN_POINT('Ctrl Pts',(-1.44488245081826,2.89183456794915,2.33193610584231));
#9900=CARTESIAN_POINT('Ctrl Pts',(-1.49120412448933,2.89574656539123,2.38281523306579));
#9901=CARTESIAN_POINT('Ctrl Pts',(-1.53482884503849,2.89965856283332,2.43613705771116));
#9902=CARTESIAN_POINT('Ctrl Pts',(-1.57550194059858,2.9035705602754,2.49157889684951));
#9903=CARTESIAN_POINT('Ctrl Pts',(-1.61621905320479,2.90748679134096,2.5470807359942));
#9904=CARTESIAN_POINT('Ctrl Pts',(-1.65397787595341,2.91140302240651,2.60470677256771));
#9905=CARTESIAN_POINT('Ctrl Pts',(-1.68856643707487,2.91531925347206,2.66410438515262));
#9906=CARTESIAN_POINT('Ctrl Pts',(-1.7231761825105,2.91923788309559,2.72353837674968));
#9907=CARTESIAN_POINT('Ctrl Pts',(-1.75461157795402,2.92315651271912,2.78474566821658));
#9908=CARTESIAN_POINT('Ctrl Pts',(-1.7827073987967,2.92707514234265,2.84735051306922));
#9909=CARTESIAN_POINT('Ctrl Pts',(-1.81085154643919,2.93100051228641,2.91006304268471));
#9910=CARTESIAN_POINT('Ctrl Pts',(-1.83564447823671,2.93492588223016,2.97417746692706));
#9911=CARTESIAN_POINT('Ctrl Pts',(-1.85697002178243,2.93885125217391,3.03930044742743));
#9912=CARTESIAN_POINT('Ctrl Pts',(-1.86649346527689,2.94060422221071,3.06838270850352));
#9913=CARTESIAN_POINT('Ctrl Pts',(-1.87532608795658,2.94235719224752,3.0976659397136));
#9914=CARTESIAN_POINT('Ctrl Pts',(-1.88346084202322,2.94411016228432,3.1271144892676));
#9915=CARTESIAN_POINT('Ctrl Pts',(-1.90162139336457,2.9480236060212,3.19285733677376));
#9916=CARTESIAN_POINT('Ctrl Pts',(-1.91637244034916,2.95193704975809,3.25968545217464));
#9917=CARTESIAN_POINT('Ctrl Pts',(-1.92758891674177,2.95585049349497,3.32721175786013));
#9918=CARTESIAN_POINT('Ctrl Pts',(-1.9387882931745,2.9597579710328,3.39463511703396));
#9919=CARTESIAN_POINT('Ctrl Pts',(-1.94646371236131,2.96366544857062,3.46275407167371));
#9920=CARTESIAN_POINT('Ctrl Pts',(-1.95054027558794,2.96757292610845,3.53116782198737));
#9921=CARTESIAN_POINT('Ctrl Pts',(-1.95461195960121,2.97147572681053,3.59949968830557));
#9922=CARTESIAN_POINT('Ctrl Pts',(-1.95509331260624,2.97537852751261,3.66812515965355));
#9923=CARTESIAN_POINT('Ctrl Pts',(-1.95196102673354,2.97928132821469,3.73663655540286));
#9924=CARTESIAN_POINT('Ctrl Pts',(-1.94883074188931,2.98318163565287,3.8051041833548));
#9925=CARTESIAN_POINT('Ctrl Pts',(-1.94209141961327,2.98708194309104,3.87345738869428));
#9926=CARTESIAN_POINT('Ctrl Pts',(-1.93177183353249,2.99098225052921,3.94128829804304));
#9927=CARTESIAN_POINT('Ctrl Pts',(-1.92145527712735,2.99488141289564,4.00909929325458));
#9928=CARTESIAN_POINT('Ctrl Pts',(-1.90756061749005,2.99878057526207,4.07638780946985));
#9929=CARTESIAN_POINT('Ctrl Pts',(-1.89016829610917,3.0026797376285,4.14275273497955));
#9930=CARTESIAN_POINT('Ctrl Pts',(-1.87277507622576,3.00657910142907,4.20912108895934));
#9931=CARTESIAN_POINT('Ctrl Pts',(-1.8518839634225,3.01047846522964,4.27456528104632));
#9932=CARTESIAN_POINT('Ctrl Pts',(-1.82762570351912,3.01437782903021,4.33869779377583));
#9933=CARTESIAN_POINT('Ctrl Pts',(-1.80334169593423,3.0182813316098,4.40289837666036));
#9934=CARTESIAN_POINT('Ctrl Pts',(-1.77568358378601,3.0221848341894,4.46578403956177));
#9935=CARTESIAN_POINT('Ctrl Pts',(-1.74483050183565,3.02608833676899,4.52698671464804));
#9936=CARTESIAN_POINT('Ctrl Pts',(-1.7139590360075,3.02999416525931,4.58822585748494));
#9937=CARTESIAN_POINT('Ctrl Pts',(-1.67988905689824,3.03389999374963,4.64777958873407));
#9938=CARTESIAN_POINT('Ctrl Pts',(-1.64284456515466,3.03780582223995,4.70530643756194));
#9939=CARTESIAN_POINT('Ctrl Pts',(-1.60573593719212,3.04171841300611,4.76293288431649));
#9940=CARTESIAN_POINT('Ctrl Pts',(-1.56564280702322,3.04563100377227,4.81852504529715));
#9941=CARTESIAN_POINT('Ctrl Pts',(-1.52283064471853,3.04954359453842,4.87177301575445));
#9942=CARTESIAN_POINT('Ctrl Pts',(-1.50242678382174,3.05140829731074,4.89715048149687));
#9943=CARTESIAN_POINT('Ctrl Pts',(-1.48140588582237,3.05327300008307,4.92199601484893));
#9944=CARTESIAN_POINT('Ctrl Pts',(-1.45979955695045,3.05513770285539,4.94627908730408));
#9945=CARTESIAN_POINT('Ctrl Pts',(-1.41438376966936,3.05905724628881,4.99732130089307));
#9946=CARTESIAN_POINT('Ctrl Pts',(-1.36619821726608,3.06297678972223,5.04607926715034));
#9947=CARTESIAN_POINT('Ctrl Pts',(-1.31550159430479,3.06689633315565,5.09223755851255));
#9948=CARTESIAN_POINT('Ctrl Pts',(-1.26488111481419,3.07080998965572,5.13832652272237));
#9949=CARTESIAN_POINT('Ctrl Pts',(-1.21175741053956,3.07472364615579,5.18182323319362));
#9950=CARTESIAN_POINT('Ctrl Pts',(-1.15642783819742,3.07863730265586,5.22244705630817));
#9951=CARTESIAN_POINT('Ctrl Pts',(-1.10116315425486,3.08254636936974,5.2630232373616));
#9952=CARTESIAN_POINT('Ctrl Pts',(-1.04369813440811,3.08645543608362,5.30073293304388));
#9953=CARTESIAN_POINT('Ctrl Pts',(-0.984363832718973,3.0903645027975,5.33533517957524));
#9954=CARTESIAN_POINT('Ctrl Pts',(-0.925066609102487,3.09427112673115,5.36991580312336));
#9955=CARTESIAN_POINT('Ctrl Pts',(-0.863902844489848,3.09817775066479,5.40139258262396));
#9956=CARTESIAN_POINT('Ctrl Pts',(-0.801231943442468,3.10208437459844,5.42956824567131));
#9957=CARTESIAN_POINT('Ctrl Pts',(-0.738578754873705,3.10598989441531,5.45773594552009));
#9958=CARTESIAN_POINT('Ctrl Pts',(-0.67441972353548,3.10989541423219,5.4826041796896));
#9959=CARTESIAN_POINT('Ctrl Pts',(-0.609136553961639,3.11380093404906,5.50402277212601));
#9960=CARTESIAN_POINT('Ctrl Pts',(-0.543849491170423,3.11770668677493,5.52544264187841));
#9961=CARTESIAN_POINT('Ctrl Pts',(-0.477438624815021,3.12161243950081,5.54341231069829));
#9962=CARTESIAN_POINT('Ctrl Pts',(-0.410301499895405,3.12551819222668,5.55783124535439));
#9963=CARTESIAN_POINT('Ctrl Pts',(-0.34309316134728,3.12942808785894,5.5722654744494));
#9964=CARTESIAN_POINT('Ctrl Pts',(-0.275157508270687,3.1333379834912,5.58314134960714));
#9965=CARTESIAN_POINT('Ctrl Pts',(-0.2069019859915,3.13724787912346,5.59040953981388));
#9966=CARTESIAN_POINT('Ctrl Pts',(-0.138605654105284,3.14116011246113,5.59768207563218));
#9967=CARTESIAN_POINT('Ctrl Pts',(-0.06998956321348,3.14507234579881,5.60134260730781));
#9968=CARTESIAN_POINT('Ctrl Pts',(-0.00146317179453743,3.14898457913649,
5.60139392046606));
#9969=CARTESIAN_POINT('Ctrl Pts',(0.067180811382858,3.15290352589345,5.60144532167804));
#9970=CARTESIAN_POINT('Ctrl Pts',(0.135734297357666,3.15682247265042,5.59787516888493));
#9971=CARTESIAN_POINT('Ctrl Pts',(0.203791822252832,3.16074141940738,5.59073820864039));
#9972=CARTESIAN_POINT('Ctrl Pts',(0.235189036955191,3.16254936074708,5.5874456899444));
#9973=CARTESIAN_POINT('Ctrl Pts',(0.266480827608339,3.16435730208677,5.5833947714429));
#9974=CARTESIAN_POINT('Ctrl Pts',(0.297628256975104,3.16616524342647,5.57859446327402));
#9975=CARTESIAN_POINT('Ctrl Pts',(0.365149803826224,3.17008450733859,5.56818833218988));
#9976=CARTESIAN_POINT('Ctrl Pts',(0.432257843245372,3.17400377125071,5.55421627178064));
#9977=CARTESIAN_POINT('Ctrl Pts',(0.498547063155325,3.17792303516283,5.53672419753157));
#9978=CARTESIAN_POINT('Ctrl Pts',(0.564736937701917,3.18183642540955,5.51925833804978));
#9979=CARTESIAN_POINT('Ctrl Pts',(0.630109956738292,3.18574981565627,5.49828305905186));
#9980=CARTESIAN_POINT('Ctrl Pts',(0.694269029376427,3.18966320590299,5.47389563577562));
#9981=CARTESIAN_POINT('Ctrl Pts',(0.758353199621903,3.19357202746938,5.44953668355233));
#9982=CARTESIAN_POINT('Ctrl Pts',(0.821225780809522,3.19748084903577,5.42177367228877));
#9983=CARTESIAN_POINT('Ctrl Pts',(0.882504692402788,3.20138967060216,5.39075371636989));
#9984=CARTESIAN_POINT('Ctrl Pts',(0.943745516642623,3.20529606267585,5.35975304062414));
#9985=CARTESIAN_POINT('Ctrl Pts',(1.00339419865734,3.20920245474955,5.32549965745886));
#9986=CARTESIAN_POINT('Ctrl Pts',(1.06108995211054,3.21310884682324,5.28818821325307));
#9987=CARTESIAN_POINT('Ctrl Pts',(1.11876960040286,3.21701414846879,5.25088718414328));
#9988=CARTESIAN_POINT('Ctrl Pts',(1.17449698980804,3.22091945011435,5.21053005545053));
#9989=CARTESIAN_POINT('Ctrl Pts',(1.22793877375832,3.22482475175991,5.1673557730219));
#9990=CARTESIAN_POINT('Ctrl Pts',(1.28138393793849,3.2287303004185,5.12417875978995));
#9991=CARTESIAN_POINT('Ctrl Pts',(1.33254282891518,3.2326358490771,5.07818454995102));
#9992=CARTESIAN_POINT('Ctrl Pts',(1.38111518643653,3.23654139773569,5.02965234646521));
#9993=CARTESIAN_POINT('Ctrl Pts',(1.42973935265201,3.24045111216647,4.98106837711474));
#9994=CARTESIAN_POINT('Ctrl Pts',(1.4757711312666,3.24436082659725,4.92994135975646));
#9995=CARTESIAN_POINT('Ctrl Pts',(1.51894788216805,3.24827054102802,4.87658661406792));
#9996=CARTESIAN_POINT('Ctrl Pts',(1.56215059095571,3.25218260598125,4.82319979147714));
#9997=CARTESIAN_POINT('Ctrl Pts',(1.60249456730862,3.25609467093448,4.7675829729797));
#9998=CARTESIAN_POINT('Ctrl Pts',(1.63975984437483,3.26000673588771,4.71008146489945));
#9999=CARTESIAN_POINT('Ctrl Pts',(1.67708927762243,3.26392553588139,4.65248096179022));
#10000=CARTESIAN_POINT('Ctrl Pts',(1.71132918811499,3.26784433587508,4.59298971906681));
#10001=CARTESIAN_POINT('Ctrl Pts',(1.74230541245396,3.27176313586877,4.53197790116833));
#10002=CARTESIAN_POINT('Ctrl Pts',(1.75661166256366,3.27357301857836,4.50379982765775));
#10003=CARTESIAN_POINT('Ctrl Pts',(1.77022243794752,3.27538290128796,4.47529769357851));
#10004=CARTESIAN_POINT('Ctrl Pts',(1.78312412104051,3.27719278399755,4.44650920908366));
#10005=CARTESIAN_POINT('Ctrl Pts',(1.81367060805643,3.28147792712892,4.37834856201985));
#10006=CARTESIAN_POINT('Ctrl Pts',(1.84034342649058,3.28576307026028,4.3083488830867));
#10007=CARTESIAN_POINT('Ctrl Pts',(1.8629392632891,3.29004821339165,4.2369479444808));
#10008=CARTESIAN_POINT('Ctrl Pts',(1.88547113914471,3.29432122677551,4.16574911706015));
#10009=CARTESIAN_POINT('Ctrl Pts',(1.903948906458,3.29859424015936,4.09315724465514));
#10010=CARTESIAN_POINT('Ctrl Pts',(1.9182171352479,3.30286725354322,4.0196296386283));
#10011=CARTESIAN_POINT('Ctrl Pts',(1.93241976769603,3.30712062229911,3.94644006628769));
#10012=CARTESIAN_POINT('Ctrl Pts',(1.94245134242074,3.311373991055,3.87232365766408));
#10013=CARTESIAN_POINT('Ctrl Pts',(1.9482066680862,3.31562735981089,3.79774997508184));
#10014=CARTESIAN_POINT('Ctrl Pts',(1.95204184265101,3.31846167581933,3.74805633352817));
#10015=CARTESIAN_POINT('Ctrl Pts',(1.95397914847566,3.32129599182777,3.6981600165373));
#10016=CARTESIAN_POINT('Ctrl Pts',(1.95399983251307,3.3241303078362,3.64820350405597));
#10017=CARTESIAN_POINT('Origin',(0.,0.,3.64739446828387));
#10018=CARTESIAN_POINT('',(1.95399924590383,4.12586969212423,3.64567778332304));
#10019=CARTESIAN_POINT('',(1.95399922086733,4.02413030792419,3.64564951846532));
#10020=CARTESIAN_POINT('',(1.954,4.33875158023511E-16,3.64739446828387));
#10021=CARTESIAN_POINT('Ctrl Pts',(1.95399924590383,4.12586969212423,3.64567778332304));
#10022=CARTESIAN_POINT('Ctrl Pts',(1.95405905160708,4.12199411980701,3.71375101849606));
#10023=CARTESIAN_POINT('Ctrl Pts',(1.95055728305734,4.11811854748978,3.78189644852607));
#10024=CARTESIAN_POINT('Ctrl Pts',(1.94349799785706,4.11424297517256,3.84970989608312));
#10025=CARTESIAN_POINT('Ctrl Pts',(1.93644199829586,4.1103692066827,3.91749178088177));
#10026=CARTESIAN_POINT('Ctrl Pts',(1.92583181766028,4.10649543819285,3.98494149260626));
#10027=CARTESIAN_POINT('Ctrl Pts',(1.91172349358429,4.10262166970299,4.05165834754822));
#10028=CARTESIAN_POINT('Ctrl Pts',(1.89761670747935,4.09874832349886,4.11836792957879));
#10029=CARTESIAN_POINT('Ctrl Pts',(1.88001263979034,4.09487497729472,4.1843443241814));
#10030=CARTESIAN_POINT('Ctrl Pts',(1.85901836975731,4.09100163109058,4.24919734373801));
#10031=CARTESIAN_POINT('Ctrl Pts',(1.83800398835006,4.08712457443046,4.31411248897668));
#10032=CARTESIAN_POINT('Ctrl Pts',(1.81359307231295,4.08324751777033,4.37790163250655));
#10033=CARTESIAN_POINT('Ctrl Pts',(1.78594218915486,4.07937046111021,4.44019109857233));
#10034=CARTESIAN_POINT('Ctrl Pts',(1.75827826652902,4.07549157612673,4.50250993879877));
#10035=CARTESIAN_POINT('Ctrl Pts',(1.72737156188945,4.07161269114325,4.56332724688238));
#10036=CARTESIAN_POINT('Ctrl Pts',(1.69342499635001,4.06773380615978,4.622293325467));
#10037=CARTESIAN_POINT('Ctrl Pts',(1.65941549088065,4.06384772938105,4.6813687323679));
#10038=CARTESIAN_POINT('Ctrl Pts',(1.62235514002204,4.05996165260232,4.73858563361944));
#10039=CARTESIAN_POINT('Ctrl Pts',(1.58249024166095,4.05607557582359,4.79362334379167));
#10040=CARTESIAN_POINT('Ctrl Pts',(1.54929063553274,4.05283923950412,4.83945891280191));
#10041=CARTESIAN_POINT('Ctrl Pts',(1.514146763539,4.04960290318465,4.88378353901681));
#10042=CARTESIAN_POINT('Ctrl Pts',(1.47722071628238,4.04636656686519,4.92643119777453));
#10043=CARTESIAN_POINT('Ctrl Pts',(1.43251138708057,4.04244807472577,4.97806814125332));
#10044=CARTESIAN_POINT('Ctrl Pts',(1.38500289026924,4.03852958258635,5.02746012816026));
#10045=CARTESIAN_POINT('Ctrl Pts',(1.33494940519801,4.03461109044694,5.07428832753251));
#10046=CARTESIAN_POINT('Ctrl Pts',(1.28497117715546,4.0306984898868,5.12104611919712));
#10047=CARTESIAN_POINT('Ctrl Pts',(1.23245591134347,4.02678588932666,5.16524744040498));
#10048=CARTESIAN_POINT('Ctrl Pts',(1.17769692864332,4.02287328876652,5.20660771356628));
#10049=CARTESIAN_POINT('Ctrl Pts',(1.12300220412355,4.01896527953697,5.24791945156929));
#10050=CARTESIAN_POINT('Ctrl Pts',(1.06606938237354,4.01505727030743,5.28639646773842));
#10051=CARTESIAN_POINT('Ctrl Pts',(1.0072260265981,4.01114926107788,5.3217933847143));
#10052=CARTESIAN_POINT('Ctrl Pts',(0.948419456670251,4.00724369493524,5.35716817335342));
#10053=CARTESIAN_POINT('Ctrl Pts',(0.887705142447654,4.0033381287926,5.38946642953763));
#10054=CARTESIAN_POINT('Ctrl Pts',(0.825439595234405,3.99943256264996,5.4184860736559));
#10055=CARTESIAN_POINT('Ctrl Pts',(0.76319162922557,3.99552809927698,5.44749752383196));
#10056=CARTESIAN_POINT('Ctrl Pts',(0.699393745278743,3.99162363590401,5.47323199209065));
#10057=CARTESIAN_POINT('Ctrl Pts',(0.634425395957633,3.98771917253103,5.49553418620673));
#10058=CARTESIAN_POINT('Ctrl Pts',(0.569453121200777,3.98381447324749,5.51783772783789));
#10059=CARTESIAN_POINT('Ctrl Pts',(0.503310706621938,3.97990977396395,5.53670842637455));
#10060=CARTESIAN_POINT('Ctrl Pts',(0.436394118017655,3.97600507468041,5.55204041274693));
#10061=CARTESIAN_POINT('Ctrl Pts',(0.369406327617285,3.97209622064828,5.56738871293611));
#10062=CARTESIAN_POINT('Ctrl Pts',(0.301643199517571,3.96818736661615,5.57919067659138));
#10063=CARTESIAN_POINT('Ctrl Pts',(0.233511292378915,3.96427851258401,5.58739149826395));
#10064=CARTESIAN_POINT('Ctrl Pts',(0.165338546892023,3.96036731558001,5.59559723551904));
#10065=CARTESIAN_POINT('Ctrl Pts',(0.0967970731610387,3.956456118576,5.60019750197605));
#10066=CARTESIAN_POINT('Ctrl Pts',(0.028296142099444,3.952544921572,5.60118957738367));
#10067=CARTESIAN_POINT('Ctrl Pts',(-0.0403227014498265,3.94862699211981,
5.60218336047726));
#10068=CARTESIAN_POINT('Ctrl Pts',(-0.108900371926817,3.94470906266763,
5.59955657561388));
#10069=CARTESIAN_POINT('Ctrl Pts',(-0.177030896040787,3.94079113321544,
5.59335851261948));
#10070=CARTESIAN_POINT('Ctrl Pts',(-0.208633889969856,3.93897376424167,
5.59048348193784));
#10071=CARTESIAN_POINT('Ctrl Pts',(-0.240140795167361,3.93715639526789,
5.58684076103463));
#10072=CARTESIAN_POINT('Ctrl Pts',(-0.271511933329573,3.93533902629411,
5.58243898199916));
#10073=CARTESIAN_POINT('Ctrl Pts',(-0.339152417294976,3.93142052909792,
5.57294814163728));
#10074=CARTESIAN_POINT('Ctrl Pts',(-0.40642843104342,3.92750203190173,5.55988765115014));
#10075=CARTESIAN_POINT('Ctrl Pts',(-0.472934213080374,3.92358353470554,
5.54329774379611));
#10076=CARTESIAN_POINT('Ctrl Pts',(-0.539340002519933,3.91967092903788,
5.52673277965569));
#10077=CARTESIAN_POINT('Ctrl Pts',(-0.604977385279366,3.91575832337022,
5.50664904841401));
#10078=CARTESIAN_POINT('Ctrl Pts',(-0.669448099005873,3.91184571770256,
5.48313825289474));
#10079=CARTESIAN_POINT('Ctrl Pts',(-0.733843159012434,3.90793770331606,
5.45965504632302));
#10080=CARTESIAN_POINT('Ctrl Pts',(-0.797073809109829,3.90402968892957,
5.4327529300141));
#10081=CARTESIAN_POINT('Ctrl Pts',(-0.858756100669926,3.90012167454307,
5.4025736498953));
#10082=CARTESIAN_POINT('Ctrl Pts',(-0.920399832111471,3.89621610321591,
5.37241323607654));
#10083=CARTESIAN_POINT('Ctrl Pts',(-0.980496684385748,3.89231053188874,
5.33897993808291));
#10084=CARTESIAN_POINT('Ctrl Pts',(-1.03868333861991,3.88840496056158,5.30246332548389));
#10085=CARTESIAN_POINT('Ctrl Pts',(-1.09685356367207,3.88450049198457,5.26595702346353));
#10086=CARTESIAN_POINT('Ctrl Pts',(-1.15311424506699,3.88059602340757,5.2263693964088));
#10087=CARTESIAN_POINT('Ctrl Pts',(-1.20712888640225,3.87669155483056,5.18393468956455));
#10088=CARTESIAN_POINT('Ctrl Pts',(-1.26114679149635,3.87278685033153,5.14149741866273));
#10089=CARTESIAN_POINT('Ctrl Pts',(-1.31291800198358,3.86888214583249,5.09621303225255));
#10090=CARTESIAN_POINT('Ctrl Pts',(-1.36213854850426,3.86497744133346,5.04835648585562));
#10091=CARTESIAN_POINT('Ctrl Pts',(-1.4114114672533,3.86106858210453,5.00044901856988));
#10092=CARTESIAN_POINT('Ctrl Pts',(-1.45812795256841,3.85715972287561,4.9499642728998));
#10093=CARTESIAN_POINT('Ctrl Pts',(-1.50202115528851,3.85325086364669,4.8972138348588));
#10094=CARTESIAN_POINT('Ctrl Pts',(-1.54594066757739,3.84933966144905,4.84443177822558));
#10095=CARTESIAN_POINT('Ctrl Pts',(-1.58703323512614,3.84542845925141,4.78938172056153));
#10096=CARTESIAN_POINT('Ctrl Pts',(-1.62507426724822,3.84151725705377,4.73240581657829));
#10097=CARTESIAN_POINT('Ctrl Pts',(-1.66318077975211,3.83759932246748,4.67533183944249));
#10098=CARTESIAN_POINT('Ctrl Pts',(-1.69822502260319,3.83368138788118,4.61632582249903));
#10099=CARTESIAN_POINT('Ctrl Pts',(-1.73002786493552,3.82976345329488,4.55575540235504));
#10100=CARTESIAN_POINT('Ctrl Pts',(-1.74477952053953,3.82794613077093,4.52765998973696));
#10101=CARTESIAN_POINT('Ctrl Pts',(-1.75883445140532,3.82612880824699,4.49922828152494));
#10102=CARTESIAN_POINT('Ctrl Pts',(-1.77217835395763,3.82431148572304,4.47049827811835));
#10103=CARTESIAN_POINT('Ctrl Pts',(-1.80095022580009,3.82039300905922,4.40855118484428));
#10104=CARTESIAN_POINT('Ctrl Pts',(-1.82652701787644,3.8164745323954,4.34497116695147));
#10105=CARTESIAN_POINT('Ctrl Pts',(-1.84872211032283,3.81255605573158,4.28012075887366));
#10106=CARTESIAN_POINT('Ctrl Pts',(-1.87088383166217,3.80864347063612,4.21536785567966));
#10107=CARTESIAN_POINT('Ctrl Pts',(-1.88967378643487,3.80473088554065,4.1493488147063));
#10108=CARTESIAN_POINT('Ctrl Pts',(-1.90495264280262,3.80081830044519,4.08244783130882));
#10109=CARTESIAN_POINT('Ctrl Pts',(-1.92021357012784,3.79691030659025,4.01562535317036));
#10110=CARTESIAN_POINT('Ctrl Pts',(-1.93197147273751,3.79300231273531,3.94792346515413));
#10111=CARTESIAN_POINT('Ctrl Pts',(-1.94013681071579,3.78909431888038,3.87974152702479));
#10112=CARTESIAN_POINT('Ctrl Pts',(-1.94829704425871,3.78518876804765,3.81160221178471));
#10113=CARTESIAN_POINT('Ctrl Pts',(-1.95286910989962,3.78128321721492,3.74298392892437));
#10114=CARTESIAN_POINT('Ctrl Pts',(-1.95381482691184,3.7773776663822,3.6742946939234));
#10115=CARTESIAN_POINT('Ctrl Pts',(-1.95476027691291,3.77347321823198,3.60562485245253));
#10116=CARTESIAN_POINT('Ctrl Pts',(-1.95208140407651,3.76956877008176,3.53688459010394));
#10117=CARTESIAN_POINT('Ctrl Pts',(-1.94579210753576,3.76566432193154,3.46848366857752));
#10118=CARTESIAN_POINT('Ctrl Pts',(-1.93950243081286,3.76175963776104,3.40007861227875));
#10119=CARTESIAN_POINT('Ctrl Pts',(-1.92960194468175,3.75785495359055,3.33201342699231));
#10120=CARTESIAN_POINT('Ctrl Pts',(-1.91615639730603,3.75395026942005,3.26469267698523));
#10121=CARTESIAN_POINT('Ctrl Pts',(-1.90269654238134,3.75004143023389,3.19730029025706));
#10122=CARTESIAN_POINT('Ctrl Pts',(-1.88568419438451,3.74613259104773,3.13065440286264));
#10123=CARTESIAN_POINT('Ctrl Pts',(-1.86523601993762,3.74222375186157,3.06514830906317));
#10124=CARTESIAN_POINT('Ctrl Pts',(-1.84477558809876,3.73831256957264,2.99960294848852));
#10125=CARTESIAN_POINT('Ctrl Pts',(-1.82087540201023,3.73440138728372,2.93519920237455));
#10126=CARTESIAN_POINT('Ctrl Pts',(-1.79370074809983,3.73049020499479,2.87231148803844));
#10127=CARTESIAN_POINT('Ctrl Pts',(-1.76647931509474,3.72657228990378,2.8093155172972));
#10128=CARTESIAN_POINT('Ctrl Pts',(-1.73597238288092,3.72265437481276,2.74784122711604));
#10129=CARTESIAN_POINT('Ctrl Pts',(-1.70239132559573,3.71873645972175,2.68823870693099));
#10130=CARTESIAN_POINT('Ctrl Pts',(-1.68681320986639,3.71691895486515,2.66058934052428));
#10131=CARTESIAN_POINT('Ctrl Pts',(-1.67057415673792,3.71510145000855,2.63334236909012));
#10132=CARTESIAN_POINT('Ctrl Pts',(-1.65369831032235,3.71328394515195,2.60653045294036));
#10133=CARTESIAN_POINT('Ctrl Pts',(-1.61731435401473,3.70936544437499,2.54872454728717));
#10134=CARTESIAN_POINT('Ctrl Pts',(-1.57782384186812,3.70544694359802,2.49271435131032));
#10135=CARTESIAN_POINT('Ctrl Pts',(-1.53542980063064,3.70152844282106,2.43885347711504));
#10136=CARTESIAN_POINT('Ctrl Pts',(-1.4930995010845,3.69761583371801,2.38507358560312));
#10137=CARTESIAN_POINT('Ctrl Pts',(-1.44787463843241,3.69370322461497,2.33343698552257));
#10138=CARTESIAN_POINT('Ctrl Pts',(-1.40000211194091,3.68979061551192,2.2842693505632));
#10139=CARTESIAN_POINT('Ctrl Pts',(-1.35218576462597,3.68588259791832,2.23515941461092));
#10140=CARTESIAN_POINT('Ctrl Pts',(-1.30172826565808,3.68197458032472,2.18851304019544));
#10141=CARTESIAN_POINT('Ctrl Pts',(-1.24891629228561,3.67806656273112,2.14462233157666));
#10142=CARTESIAN_POINT('Ctrl Pts',(-1.19613733574055,3.67416098833996,2.10075906241637));
#10143=CARTESIAN_POINT('Ctrl Pts',(-1.14100720208999,3.6702554139488,2.05964835518215));
#10144=CARTESIAN_POINT('Ctrl Pts',(-1.0838477331168,3.66634983955765,2.02154389353305));
#10145=CARTESIAN_POINT('Ctrl Pts',(-1.02670440542699,3.66244536806307,1.98345019221683));
#10146=CARTESIAN_POINT('Ctrl Pts',(-0.967533289053187,3.6585408965685,1.94836132382118));
#10147=CARTESIAN_POINT('Ctrl Pts',(-0.906685980488979,3.65463642507392,
1.91648819329821));
#10148=CARTESIAN_POINT('Ctrl Pts',(-0.845834997649865,3.65073171780719,
1.88461313811092));
#10149=CARTESIAN_POINT('Ctrl Pts',(-0.783308058478771,3.64682701054045,
1.85595443221954));
#10150=CARTESIAN_POINT('Ctrl Pts',(-0.719480558857405,3.64292230327371,
1.8306766240862));
#10151=CARTESIAN_POINT('Ctrl Pts',(-0.655585148751602,3.63901344151927,
1.80537192114723));
#10152=CARTESIAN_POINT('Ctrl Pts',(-0.590386874763926,3.63510457976483,
1.78345547613733));
#10153=CARTESIAN_POINT('Ctrl Pts',(-0.524279328070026,3.63119571801039,
1.76504296387285));
#10154=CARTESIAN_POINT('Ctrl Pts',(-0.458132158838919,3.62728451342177,
1.74661941579644));
#10155=CARTESIAN_POINT('Ctrl Pts',(-0.391075112364722,3.62337330883315,
1.73170408691508));
#10156=CARTESIAN_POINT('Ctrl Pts',(-0.323512339793095,3.61946210424453,
1.72036157650397));
#10157=CARTESIAN_POINT('Ctrl Pts',(-0.255833274830453,3.61554416749681,
1.70899954280207));
#10158=CARTESIAN_POINT('Ctrl Pts',(-0.1876472347705,3.6116262307491,1.70122265691393));
#10159=CARTESIAN_POINT('Ctrl Pts',(-0.119362978636752,3.60770829400139,
1.69704360771263));
#10160=CARTESIAN_POINT('Ctrl Pts',(-0.0876899972033133,3.60589099752789,
1.69510519679251));
#10161=CARTESIAN_POINT('Ctrl Pts',(-0.0559958742506681,3.60407370105439,
1.69394011591222));
#10162=CARTESIAN_POINT('Ctrl Pts',(-0.0243211323379373,3.60225640458088,
1.69354583481151));
#10163=CARTESIAN_POINT('Ctrl Pts',(0.0439771955415224,3.59833787824392,
1.69269567035027));
#10164=CARTESIAN_POINT('Ctrl Pts',(0.112455204635595,3.59441935190696,1.69542926853147));
#10165=CARTESIAN_POINT('Ctrl Pts',(0.180705710999457,3.59050082557,1.70176823336305));
#10166=CARTESIAN_POINT('Ctrl Pts',(0.248853606178245,3.58658819053923,1.70809766788154));
#10167=CARTESIAN_POINT('Ctrl Pts',(0.316774191731649,3.58267555550847,1.71802166608982));
#10168=CARTESIAN_POINT('Ctrl Pts',(0.384059911532946,3.57876292047771,1.73150982030704));
#10169=CARTESIAN_POINT('Ctrl Pts',(0.451266678062233,3.57485487654501,1.74498214748233));
#10170=CARTESIAN_POINT('Ctrl Pts',(0.517839578447494,3.57094683261231,1.76201022850722));
#10171=CARTESIAN_POINT('Ctrl Pts',(0.583377636205858,3.5670387886796,1.78251202330916));
#10172=CARTESIAN_POINT('Ctrl Pts',(0.648874725369101,3.5631331877102,1.80300100220291));
#10173=CARTESIAN_POINT('Ctrl Pts',(0.713337786868064,3.55922758674079,1.82695924084991));
#10174=CARTESIAN_POINT('Ctrl Pts',(0.776379002836208,3.55532198577139,1.85425430534204));
#10175=CARTESIAN_POINT('Ctrl Pts',(0.839402419871464,3.55141748750168,1.88154166339936));
#10176=CARTESIAN_POINT('Ctrl Pts',(0.901004337256454,3.54751298923197,1.91216378171598));
#10177=CARTESIAN_POINT('Ctrl Pts',(0.960816693257145,3.54360849096226,1.94594000754788));
#10178=CARTESIAN_POINT('Ctrl Pts',(1.02063266338498,3.53970375676549,1.97971827428876));
#10179=CARTESIAN_POINT('Ctrl Pts',(1.07865843051714,3.53579902256872,2.01665078287664));
#10180=CARTESIAN_POINT('Ctrl Pts',(1.13455192769971,3.53189428837195,2.05651171856507));
#10181=CARTESIAN_POINT('Ctrl Pts',(1.19050489408076,3.52798539964157,2.09641506523179));
#10182=CARTESIAN_POINT('Ctrl Pts',(1.24432066185116,3.52407651091118,2.13925277096345));
#10183=CARTESIAN_POINT('Ctrl Pts',(1.29568831620735,3.5201676221808,2.18475719703588));
#10184=CARTESIAN_POINT('Ctrl Pts',(1.34708675917241,3.51625639055102,2.23028889743092));
#10185=CARTESIAN_POINT('Ctrl Pts',(1.39603381800536,3.51234515892124,2.27849015414639));
#10186=CARTESIAN_POINT('Ctrl Pts',(1.44225572602455,3.50843392729146,2.32905671916592));
#10187=CARTESIAN_POINT('Ctrl Pts',(1.48855719073511,3.50451596368844,2.37971031885751));
#10188=CARTESIAN_POINT('Ctrl Pts',(1.53212383128939,3.50059800008543,2.43273697234043));
#10189=CARTESIAN_POINT('Ctrl Pts',(1.57272296308911,3.49668003648242,2.48780036629291));
#10190=CARTESIAN_POINT('Ctrl Pts',(1.59155186606893,3.49486297899154,2.51333744692767));
#10191=CARTESIAN_POINT('Ctrl Pts',(1.60974311680235,3.49304592150067,2.53931221537671));
#10192=CARTESIAN_POINT('Ctrl Pts',(1.62727683669187,3.4912288640098,2.5656892881326));
#10193=CARTESIAN_POINT('Ctrl Pts',(1.66576335091087,3.48724042291459,2.6235869614199));
#10194=CARTESIAN_POINT('Ctrl Pts',(1.70122719124069,3.48325198181939,2.68364762603427));
#10195=CARTESIAN_POINT('Ctrl Pts',(1.73342304991814,3.47926354072418,2.74552943957254));
#10196=CARTESIAN_POINT('Ctrl Pts',(1.76556540124553,3.47528172814962,2.8073084097019));
#10197=CARTESIAN_POINT('Ctrl Pts',(1.79445034260505,3.47129991557505,2.87090210568559));
#10198=CARTESIAN_POINT('Ctrl Pts',(1.81987604929994,3.46731810300049,2.93594020750215));
#10199=CARTESIAN_POINT('Ctrl Pts',(1.84526035100446,3.46334277468665,3.00087239674718));
#10200=CARTESIAN_POINT('Ctrl Pts',(1.86719645127401,3.45936744637281,3.06724388003212));
#10201=CARTESIAN_POINT('Ctrl Pts',(1.8855294599692,3.45539211805897,3.13466193022113));
#10202=CARTESIAN_POINT('Ctrl Pts',(1.90384492772801,3.45142059332054,3.20201547513723));
#10203=CARTESIAN_POINT('Ctrl Pts',(1.91856402806963,3.44744906858211,3.2704131477722));
#10204=CARTESIAN_POINT('Ctrl Pts',(1.92958115826743,3.44347754384368,3.3394455217695));
#10205=CARTESIAN_POINT('Ctrl Pts',(1.94059067635588,3.43950876316655,3.40843019895554));
#10206=CARTESIAN_POINT('Ctrl Pts',(1.94790323385188,3.43553998248942,3.47804824402431));
#10207=CARTESIAN_POINT('Ctrl Pts',(1.95146428769477,3.43157120181229,3.54787997762083));
#10208=CARTESIAN_POINT('Ctrl Pts',(1.95316954552555,3.42967069858293,3.58131982880137));
#10209=CARTESIAN_POINT('Ctrl Pts',(1.9540153051049,3.42777019535358,3.61480856012882));
#10210=CARTESIAN_POINT('Ctrl Pts',(1.95399979033479,3.42586969212423,3.64829965974897));
#10211=CARTESIAN_POINT('Ctrl Pts',(1.95399983251336,3.32413030787577,3.64820350335859));
#10212=CARTESIAN_POINT('Ctrl Pts',(1.95402888143147,3.32811085978268,3.57804389856128));
#10213=CARTESIAN_POINT('Ctrl Pts',(1.95027489940238,3.3320914116896,3.507903037527));
#10214=CARTESIAN_POINT('Ctrl Pts',(1.94277019996063,3.33607196359651,3.43820567760683));
#10215=CARTESIAN_POINT('Ctrl Pts',(1.93526110496938,3.34005484693764,3.36846749550601));
#10216=CARTESIAN_POINT('Ctrl Pts',(1.92399697641739,3.34403773027876,3.2991737923561));
#10217=CARTESIAN_POINT('Ctrl Pts',(1.90906168828393,3.34802061361988,3.2307417707929));
#10218=CARTESIAN_POINT('Ctrl Pts',(1.89410146887175,3.35201014553542,3.16219551656222));
#10219=CARTESIAN_POINT('Ctrl Pts',(1.87545795844452,3.35599967745097,3.09451426921879));
#10220=CARTESIAN_POINT('Ctrl Pts',(1.8532655171138,3.35998920936651,3.0281021923132));
#10221=CARTESIAN_POINT('Ctrl Pts',(1.83105197340533,3.36398253485341,2.96162696540474));
#10222=CARTESIAN_POINT('Ctrl Pts',(1.80528295013382,3.3679758603403,2.89642374334015));
#10223=CARTESIAN_POINT('Ctrl Pts',(1.77614075125037,3.37196918582719,2.83287618626205));
#10224=CARTESIAN_POINT('Ctrl Pts',(1.74693910067287,3.37597065791846,2.76919898866038));
#10225=CARTESIAN_POINT('Ctrl Pts',(1.71435075203521,3.37997213000973,2.70718460986608));
#10226=CARTESIAN_POINT('Ctrl Pts',(1.67860342342437,3.383973602101,2.64719121550573));
#10227=CARTESIAN_POINT('Ctrl Pts',(1.66595732884495,3.38538917625688,2.62596775157977));
#10228=CARTESIAN_POINT('Ctrl Pts',(1.65291627738983,3.38680475041275,2.60499692950164));
#10229=CARTESIAN_POINT('Ctrl Pts',(1.63949157496413,3.38822032456863,2.58429363787236));
#10230=CARTESIAN_POINT('Ctrl Pts',(1.60232839550314,3.39213901376762,2.5269813699461));
#10231=CARTESIAN_POINT('Ctrl Pts',(1.56208293473805,3.3960577029666,2.47150688257573));
#10232=CARTESIAN_POINT('Ctrl Pts',(1.51896302007945,3.39997639216559,2.41822102908535));
#10233=CARTESIAN_POINT('Ctrl Pts',(1.47590791688916,3.40388919137145,2.36501526699665));
#10234=CARTESIAN_POINT('Ctrl Pts',(1.42998724131847,3.40780199057731,2.31399198913328));
#10235=CARTESIAN_POINT('Ctrl Pts',(1.3814523097093,3.41171478978318,2.26547351685472));
#10236=CARTESIAN_POINT('Ctrl Pts',(1.33297431285744,3.41562299901094,2.21701196002557));
#10237=CARTESIAN_POINT('Ctrl Pts',(1.28188849665375,3.4195312082387,2.17104971919529));
#10238=CARTESIAN_POINT('Ctrl Pts',(1.2284854962011,3.42343941746646,2.12787500949976));
#10239=CARTESIAN_POINT('Ctrl Pts',(1.17511586903215,3.4273451843263,2.08472728109412));
#10240=CARTESIAN_POINT('Ctrl Pts',(1.11943231171976,3.43125095118614,2.04436393660704));
#10241=CARTESIAN_POINT('Ctrl Pts',(1.06176009971694,3.43515671804598,2.00703429726987));
#10242=CARTESIAN_POINT('Ctrl Pts',(1.00410416509047,3.43906138254412,1.96971519383149));
#10243=CARTESIAN_POINT('Ctrl Pts',(0.944461102619404,3.44296604704227,1.93542836280035));
#10244=CARTESIAN_POINT('Ctrl Pts',(0.883185360289921,3.44687071154042,1.9043799475843));
#10245=CARTESIAN_POINT('Ctrl Pts',(0.821905914294495,3.45077561204669,1.87332965572091));
#10246=CARTESIAN_POINT('Ctrl Pts',(0.758994032295715,3.45468051255296,1.84551838823025));
#10247=CARTESIAN_POINT('Ctrl Pts',(0.694827332237139,3.45858541305923,1.82110561424784));
#10248=CARTESIAN_POINT('Ctrl Pts',(0.630592380268214,3.46249446707377,1.796666873238));
#10249=CARTESIAN_POINT('Ctrl Pts',(0.565100407054043,3.46640352108831,1.77563401497833));
#10250=CARTESIAN_POINT('Ctrl Pts',(0.498746563303162,3.47031257510285,1.75811739342341));
#10251=CARTESIAN_POINT('Ctrl Pts',(0.432352956123435,3.47422397167032,1.74059027479862));
#10252=CARTESIAN_POINT('Ctrl Pts',(0.365096931931761,3.47813536823779,1.72658368679371));
#10253=CARTESIAN_POINT('Ctrl Pts',(0.297383510811573,3.48204676480526,1.71615676994185));
#10254=CARTESIAN_POINT('Ctrl Pts',(0.229553586201177,3.48596489107778,1.70571191318701));
#10255=CARTESIAN_POINT('Ctrl Pts',(0.16126518299087,3.48988301735029,1.69885906877363));
#10256=CARTESIAN_POINT('Ctrl Pts',(0.092927228014007,3.49380114362281,1.69560540942181));
#10257=CARTESIAN_POINT('Ctrl Pts',(0.0612609174780538,3.49561671746177,
1.69409773499041));
#10258=CARTESIAN_POINT('Ctrl Pts',(0.0295839467281558,3.49743229130074,
1.69336213986674));
#10259=CARTESIAN_POINT('Ctrl Pts',(-0.0020633167638207,3.49924786513971,
1.69339555765881));
#10260=CARTESIAN_POINT('Ctrl Pts',(-0.070367973775412,3.50316643928061,
1.69346768366824));
#10261=CARTESIAN_POINT('Ctrl Pts',(-0.138803851921803,3.50708501342151,
1.6971257846081));
#10262=CARTESIAN_POINT('Ctrl Pts',(-0.206963501706444,3.51100358756241,
1.70438594824043));
#10263=CARTESIAN_POINT('Ctrl Pts',(-0.275020711479259,3.51491627231299,
1.71163520026668));
#10264=CARTESIAN_POINT('Ctrl Pts',(-0.342802031772617,3.51882895706358,
1.72247571894333));
#10265=CARTESIAN_POINT('Ctrl Pts',(-0.409900345716198,3.52274164181416,
1.73687158001958));
#10266=CARTESIAN_POINT('Ctrl Pts',(-0.476919971846414,3.52664973806484,
1.75125055872184));
#10267=CARTESIAN_POINT('Ctrl Pts',(-0.543257703856739,3.53055783431552,
1.7691764965273));
#10268=CARTESIAN_POINT('Ctrl Pts',(-0.608513703120392,3.53446593056619,
1.79056193056952));
#10269=CARTESIAN_POINT('Ctrl Pts',(-0.673728937109452,3.53837158543801,
1.81193400517965));
#10270=CARTESIAN_POINT('Ctrl Pts',(-0.737863312607149,3.54227724030983,
1.8367611361605));
#10271=CARTESIAN_POINT('Ctrl Pts',(-0.800530830918342,3.54618289518165,
1.86490564959546));
#10272=CARTESIAN_POINT('Ctrl Pts',(-0.863180680188064,3.55008744885815,
1.8930422277142));
#10273=CARTESIAN_POINT('Ctrl Pts',(-0.924364044941099,3.55399200253465,
1.92449413008883));
#10274=CARTESIAN_POINT('Ctrl Pts',(-0.983715333682362,3.55789655621115,
1.95907573585264));
#10275=CARTESIAN_POINT('Ctrl Pts',(-1.04307023031463,3.56180134724061,1.99365944378924));
#10276=CARTESIAN_POINT('Ctrl Pts',(-1.1005924062468,3.56570613827007,2.03137298304475));
#10277=CARTESIAN_POINT('Ctrl Pts',(-1.15594287369403,3.56961092929953,2.07198592674425));
#10278=CARTESIAN_POINT('Ctrl Pts',(-1.21135225688763,3.57351987663857,2.11264209938112));
#10279=CARTESIAN_POINT('Ctrl Pts',(-1.26458492120614,3.57742882397761,2.15620354395487));
#10280=CARTESIAN_POINT('Ctrl Pts',(-1.31533359401799,3.58133777131664,2.2023984349164));
#10281=CARTESIAN_POINT('Ctrl Pts',(-1.36611269826737,3.58524906265564,2.24862102664054));
#10282=CARTESIAN_POINT('Ctrl Pts',(-1.41440450085397,3.58916035399463,2.29747985777431));
#10283=CARTESIAN_POINT('Ctrl Pts',(-1.45993936916702,3.59307164533362,2.34866699942976));
#10284=CARTESIAN_POINT('Ctrl Pts',(-1.5055526230006,3.59698966972398,2.39994225665228));
#10285=CARTESIAN_POINT('Ctrl Pts',(-1.54839916383633,3.60090769411435,2.45355343977756));
#10286=CARTESIAN_POINT('Ctrl Pts',(-1.58825087105825,3.60482571850471,2.50916111321879));
#10287=CARTESIAN_POINT('Ctrl Pts',(-1.60672781397214,3.60664228090674,2.53494319081025));
#10288=CARTESIAN_POINT('Ctrl Pts',(-1.62456160331133,3.60845884330876,2.56115406024028));
#10289=CARTESIAN_POINT('Ctrl Pts',(-1.64173285670969,3.61027540571079,2.58775810273207));
#10290=CARTESIAN_POINT('Ctrl Pts',(-1.67877187594956,3.61419379700106,2.64514399174383));
#10291=CARTESIAN_POINT('Ctrl Pts',(-1.7128717211391,3.61811218829132,2.70458778327013));
#10292=CARTESIAN_POINT('Ctrl Pts',(-1.74379755342956,3.62203057958159,2.76575616792874));
#10293=CARTESIAN_POINT('Ctrl Pts',(-1.77467687365945,3.62594307766092,2.82683255611057));
#10294=CARTESIAN_POINT('Ctrl Pts',(-1.80239143499207,3.62985557574025,2.88962795431011));
#10295=CARTESIAN_POINT('Ctrl Pts',(-1.82675024602297,3.63376807381959,2.95378107549578));
#10296=CARTESIAN_POINT('Ctrl Pts',(-1.85108046000917,3.63767597865821,3.01785888144244));
#10297=CARTESIAN_POINT('Ctrl Pts',(-1.87206257414133,3.64158388349683,3.08329078713669));
#10298=CARTESIAN_POINT('Ctrl Pts',(-1.88955282088807,3.64549178833545,3.14969361729612));
#10299=CARTESIAN_POINT('Ctrl Pts',(-1.90703212830283,3.64939724896221,3.21605491558839));
#10300=CARTESIAN_POINT('Ctrl Pts',(-1.9210237757486,3.65330270958898,3.28338545919602));
#10301=CARTESIAN_POINT('Ctrl Pts',(-1.93143366978043,3.65720817021575,3.35128641496802));
#10302=CARTESIAN_POINT('Ctrl Pts',(-1.94184062184129,3.66111252710872,3.41916818104986));
#10303=CARTESIAN_POINT('Ctrl Pts',(-1.94866775551529,3.6650168840017,3.48761955338133));
#10304=CARTESIAN_POINT('Ctrl Pts',(-1.9518723184559,3.66892124089468,3.55623278529381));
#10305=CARTESIAN_POINT('Ctrl Pts',(-1.95507707436364,3.67282583289383,3.62485014884563));
#10306=CARTESIAN_POINT('Ctrl Pts',(-1.95465880608775,3.67673042489298,3.69362889995227));
#10307=CARTESIAN_POINT('Ctrl Pts',(-1.95062683160632,3.68063501689213,3.7621592878825));
#10308=CARTESIAN_POINT('Ctrl Pts',(-1.94659056733331,3.68454376315513,3.83076258824859));
#10309=CARTESIAN_POINT('Ctrl Pts',(-1.93893295289844,3.68845250941814,3.89911650621308));
#10310=CARTESIAN_POINT('Ctrl Pts',(-1.92771529253688,3.69236125568115,3.96681543021258));
#10311=CARTESIAN_POINT('Ctrl Pts',(-1.91649090935577,3.69627234448217,4.03455492663406));
#10312=CARTESIAN_POINT('Ctrl Pts',(-1.9017023399559,3.70018343328319,4.10163816753876));
#10313=CARTESIAN_POINT('Ctrl Pts',(-1.88346164729895,3.7040945220842,4.16767153212));
#10314=CARTESIAN_POINT('Ctrl Pts',(-1.86518955342549,3.70801234379545,4.23381857264636));
#10315=CARTESIAN_POINT('Ctrl Pts',(-1.84345363127516,3.7119301655067,4.29891166351186));
#10316=CARTESIAN_POINT('Ctrl Pts',(-1.81841494640218,3.71584798721795,4.36257492292532));
#10317=CARTESIAN_POINT('Ctrl Pts',(-1.80679411803862,3.71766630690592,4.39212199436546));
#10318=CARTESIAN_POINT('Ctrl Pts',(-1.79446252923637,3.7194846265939,4.42136139692646));
#10319=CARTESIAN_POINT('Ctrl Pts',(-1.78143961641532,3.72130294628187,4.45025740370065));
#10320=CARTESIAN_POINT('Ctrl Pts',(-1.75337490510792,3.72522147186894,4.51252903979293));
#10321=CARTESIAN_POINT('Ctrl Pts',(-1.72198563863023,3.72913999745601,4.57345050024927));
#10322=CARTESIAN_POINT('Ctrl Pts',(-1.6874241453808,3.73305852304309,4.63264355028591));
#10323=CARTESIAN_POINT('Ctrl Pts',(-1.65291461281587,3.73697115741272,4.69174760788883));
#10324=CARTESIAN_POINT('Ctrl Pts',(-1.61524256473294,3.74088379178235,4.74912799103301));
#10325=CARTESIAN_POINT('Ctrl Pts',(-1.57460763543134,3.74479642615199,4.804428086828));
#10326=CARTESIAN_POINT('Ctrl Pts',(-1.5340203858993,3.74870446955743,4.85966329520053));
#10327=CARTESIAN_POINT('Ctrl Pts',(-1.49047744950318,3.75261251296288,4.91282266960529));
#10328=CARTESIAN_POINT('Ctrl Pts',(-1.44422248756346,3.75652055636833,4.9635773607483));
#10329=CARTESIAN_POINT('Ctrl Pts',(-1.39799643915049,3.76042615689386,5.01430032562759));
#10330=CARTESIAN_POINT('Ctrl Pts',(-1.34906205859251,3.76433175741939,5.06262122638954));
#10331=CARTESIAN_POINT('Ctrl Pts',(-1.29770313383148,3.76823735794492,5.10824441829378));
#10332=CARTESIAN_POINT('Ctrl Pts',(-1.24635870854784,3.77214185585457,5.15385473001327));
#10333=CARTESIAN_POINT('Ctrl Pts',(-1.19259146538888,3.77604635376421,5.196768518388));
#10334=CARTESIAN_POINT('Ctrl Pts',(-1.13672056180759,3.77995085167385,5.23672840561858));
#10335=CARTESIAN_POINT('Ctrl Pts',(-1.08084628105307,3.78385558559481,5.27669070826492));
#10336=CARTESIAN_POINT('Ctrl Pts',(-1.0228684889009,3.78776031951578,5.31369847130271));
#10337=CARTESIAN_POINT('Ctrl Pts',(-0.963136307333334,3.79166505343674,
5.34753694863554));
#10338=CARTESIAN_POINT('Ctrl Pts',(-0.903340570335241,3.79557394202005,
5.3814114303288));
#10339=CARTESIAN_POINT('Ctrl Pts',(-0.841787147330356,3.79948283060335,
5.41210965379722));
#10340=CARTESIAN_POINT('Ctrl Pts',(-0.778849921474265,3.80339171918666,
5.43946277050327));
#10341=CARTESIAN_POINT('Ctrl Pts',(-0.715874971288074,3.80730295074269,
5.46683228256184));
#10342=CARTESIAN_POINT('Ctrl Pts',(-0.651515028264089,3.81121418229871,
5.49085252547173));
#10343=CARTESIAN_POINT('Ctrl Pts',(-0.586161478091735,3.81512541385474,
5.51140378199486));
#10344=CARTESIAN_POINT('Ctrl Pts',(-0.520695440139975,3.81904337749726,
5.53199041173343));
#10345=CARTESIAN_POINT('Ctrl Pts',(-0.454232857736644,3.82296134113978,
5.54909601583925));
#10346=CARTESIAN_POINT('Ctrl Pts',(-0.387176839061591,3.8268793047823,5.56265165605116));
#10347=CARTESIAN_POINT('Ctrl Pts',(-0.356077812451395,3.82869636547252,
5.56893844766209));
#10348=CARTESIAN_POINT('Ctrl Pts',(-0.324851235324715,3.83051342616273,
5.57446241188905));
#10349=CARTESIAN_POINT('Ctrl Pts',(-0.293537575865702,3.83233048685294,
5.57922046757959));
#10350=CARTESIAN_POINT('Ctrl Pts',(-0.226009535275472,3.83624898600517,
5.58948123503227));
#10351=CARTESIAN_POINT('Ctrl Pts',(-0.157809303592958,3.84016748515741,
5.59621731169598));
#10352=CARTESIAN_POINT('Ctrl Pts',(-0.0893371895893358,3.84408598430965,
5.59935114468739));
#10353=CARTESIAN_POINT('Ctrl Pts',(-0.0209680207510835,3.84799859215052,
5.60248026608256));
#10354=CARTESIAN_POINT('Ctrl Pts',(0.047671731832998,3.85191119999139,5.60201787010988));
#10355=CARTESIAN_POINT('Ctrl Pts',(0.116174217614918,3.85582380783227,5.59793786722724));
#10356=CARTESIAN_POINT('Ctrl Pts',(0.1845963240613,3.85973182470371,5.59386265173177));
#10357=CARTESIAN_POINT('Ctrl Pts',(0.252880995006168,3.86363984157514,5.5861782887665));
#10358=CARTESIAN_POINT('Ctrl Pts',(0.320619775904284,3.86754785844658,5.57491073521888));
#10359=CARTESIAN_POINT('Ctrl Pts',(0.3883162138864,3.87145343245106,5.56365022491987));
#10360=CARTESIAN_POINT('Ctrl Pts',(0.455466954707273,3.87535900645553,5.54881104769229));
#10361=CARTESIAN_POINT('Ctrl Pts',(0.52166962687112,3.87926458046,5.53047088744485));
#10362=CARTESIAN_POINT('Ctrl Pts',(0.587853609714223,3.88316905190286,5.51213590470953));
#10363=CARTESIAN_POINT('Ctrl Pts',(0.653089581535267,3.88707352334571,5.49030203224722));
#10364=CARTESIAN_POINT('Ctrl Pts',(0.71698808841942,3.89097799478857,5.46509743661084));
#10365=CARTESIAN_POINT('Ctrl Pts',(0.780890459305323,3.89488270233842,5.43989131682927));
#10366=CARTESIAN_POINT('Ctrl Pts',(0.843454748170452,3.89878740988827,5.41131425203811));
#10367=CARTESIAN_POINT('Ctrl Pts',(0.904311019378003,3.90269211743813,5.37954272413021));
#10368=CARTESIAN_POINT('Ctrl Pts',(0.965232047594523,3.90660097997771,5.34773738821737));
#10369=CARTESIAN_POINT('Ctrl Pts',(1.0244409942742,3.91050984251729,5.312731033499));
#10370=CARTESIAN_POINT('Ctrl Pts',(1.08159301051882,3.91441870505687,5.27474586229711));
#10371=CARTESIAN_POINT('Ctrl Pts',(1.13877928587347,3.91832991071854,5.23673792132706));
#10372=CARTESIAN_POINT('Ctrl Pts',(1.19390578221152,3.92224111638021,5.1957479036233));
#10373=CARTESIAN_POINT('Ctrl Pts',(1.24665939534098,3.92615232204189,5.15203939384208));
#10374=CARTESIAN_POINT('Ctrl Pts',(1.29950381638474,3.93007026029319,5.1082556460179));
#10375=CARTESIAN_POINT('Ctrl Pts',(1.34996684078175,3.93398819854449,5.0617443998175));
#10376=CARTESIAN_POINT('Ctrl Pts',(1.39777163204783,3.93790613679579,5.01280666415819));
#10377=CARTESIAN_POINT('Ctrl Pts',(1.41994541127994,3.93972343367186,4.99010737988375));
#10378=CARTESIAN_POINT('Ctrl Pts',(1.44154784196988,3.94154073054794,4.9668865155006));
#10379=CARTESIAN_POINT('Ctrl Pts',(1.46255434627851,3.94335802742402,4.94317638827729));
#10380=CARTESIAN_POINT('Ctrl Pts',(1.50741523544836,3.94723899460202,4.89254171941757));
#10381=CARTESIAN_POINT('Ctrl Pts',(1.54974101147076,3.95111996178002,4.83946434287415));
#10382=CARTESIAN_POINT('Ctrl Pts',(1.58925110793399,3.95500092895803,4.7842308311482));
#10383=CARTESIAN_POINT('Ctrl Pts',(1.62870618822605,3.95887649205015,4.72907422979723));
#10384=CARTESIAN_POINT('Ctrl Pts',(1.66535307107132,3.96275205514227,4.6717678481909));
#10385=CARTESIAN_POINT('Ctrl Pts',(1.69894984269427,3.96662761823439,4.61263300461006));
#10386=CARTESIAN_POINT('Ctrl Pts',(1.73251188796112,3.97049917545995,4.55355928409362));
#10387=CARTESIAN_POINT('Ctrl Pts',(1.76302982718898,3.97437073268551,4.49266128331332));
#10388=CARTESIAN_POINT('Ctrl Pts',(1.79030481181464,3.97824228991107,4.43028953200145));
#10389=CARTESIAN_POINT('Ctrl Pts',(1.81756762166772,3.98211211898428,4.36794562165441));
#10390=CARTESIAN_POINT('Ctrl Pts',(1.84159013640073,3.98598194805749,4.30412971952848));
#10391=CARTESIAN_POINT('Ctrl Pts',(1.86222007239024,3.9898517771307,4.23921572676222));
#10392=CARTESIAN_POINT('Ctrl Pts',(1.8828434276196,3.99372037176397,4.17432244096358));
#10393=CARTESIAN_POINT('Ctrl Pts',(1.90007620415411,3.99758896639724,4.10833223942768));
#10394=CARTESIAN_POINT('Ctrl Pts',(1.91381554134504,4.00145756103051,4.04163560478056));
#10395=CARTESIAN_POINT('Ctrl Pts',(1.9275638962301,4.00532869478213,3.97489519437901));
#10396=CARTESIAN_POINT('Ctrl Pts',(1.93781412805708,4.00919982853375,3.90744791692333));
#10397=CARTESIAN_POINT('Ctrl Pts',(1.94451449325912,4.01307096228536,3.83969471660724));
#10398=CARTESIAN_POINT('Ctrl Pts',(1.95089519540874,4.0167574108155,3.77517390649239));
#10399=CARTESIAN_POINT('Ctrl Pts',(1.95405702262766,4.02044385934563,3.71037610742826));
#10400=CARTESIAN_POINT('Ctrl Pts',(1.95399922086809,4.02413030787577,3.64564951931539));
#10401=CARTESIAN_POINT('Origin',(0.,0.,3.64739446828387));
#10402=CARTESIAN_POINT('',(1.95430222507481,4.82586969212423,3.64764326884654));
#10403=CARTESIAN_POINT('',(1.95427619993066,4.72413035081974,3.647777104142));
#10404=CARTESIAN_POINT('',(1.954,4.33875158023511E-16,3.64739446828387));
#10405=CARTESIAN_POINT('Ctrl Pts',(1.95715633972901,4.82586969212423,3.64764363220146));
#10406=CARTESIAN_POINT('Ctrl Pts',(1.95718052860821,4.8250995783704,3.66109012482265));
#10407=CARTESIAN_POINT('Ctrl Pts',(1.95096916696084,4.78732028442627,4.32070869776071));
#10408=CARTESIAN_POINT('Ctrl Pts',(1.21359828804361,4.71253181029161,5.61146159126724));
#10409=CARTESIAN_POINT('Ctrl Pts',(-0.989869636257424,4.60150426972061,
5.73318883630065));
#10410=CARTESIAN_POINT('Ctrl Pts',(-2.28894570144034,4.49047672914949,3.94923537617169));
#10411=CARTESIAN_POINT('Ctrl Pts',(-1.49673214248602,4.37944918857844,1.88950560619207));
#10412=CARTESIAN_POINT('Ctrl Pts',(0.662966995866533,4.26842164800734,1.4358667599271));
#10413=CARTESIAN_POINT('Ctrl Pts',(1.8460276791096,4.18389531480082,2.62877633203429));
#10414=CARTESIAN_POINT('Ctrl Pts',(1.95459509422112,4.13637816178466,3.46119040754886));
#10415=CARTESIAN_POINT('Ctrl Pts',(1.95303263999471,4.12587018895884,3.64566991009788));
#10416=CARTESIAN_POINT('Ctrl Pts',(1.95399922086733,4.02413030792418,3.64564951846532));
#10417=CARTESIAN_POINT('Ctrl Pts',(1.95392015614754,4.02917285126933,3.55711264524746));
#10418=CARTESIAN_POINT('Ctrl Pts',(1.94781926961924,4.03421539461449,3.46884243996873));
#10419=CARTESIAN_POINT('Ctrl Pts',(1.93583046129939,4.03925793795964,3.38154408723206));
#10420=CARTESIAN_POINT('Ctrl Pts',(1.92384165297954,4.0443004813048,3.29424573449538));
#10421=CARTESIAN_POINT('Ctrl Pts',(1.90596512136721,4.04934302464995,3.20791897386854));
#10422=CARTESIAN_POINT('Ctrl Pts',(1.88238740014386,4.05438556799511,3.12324403588909));
#10423=CARTESIAN_POINT('Ctrl Pts',(1.86406544961994,4.0583040649868,3.05744420690734));
#10424=CARTESIAN_POINT('Ctrl Pts',(1.84225301252199,4.06222256197849,2.99247609015031));
#10425=CARTESIAN_POINT('Ctrl Pts',(1.81704344396078,4.06614105897018,2.92873660618317));
#10426=CARTESIAN_POINT('Ctrl Pts',(1.79187177822554,4.0700536644644,2.86509295513607));
#10427=CARTESIAN_POINT('Ctrl Pts',(1.76331329734947,4.07396626995861,2.80267472432111));
#10428=CARTESIAN_POINT('Ctrl Pts',(1.73151138885157,4.07787887545283,2.74186461771168));
#10429=CARTESIAN_POINT('Ctrl Pts',(1.69974679820311,4.08178688971244,2.68112586853045));
#10430=CARTESIAN_POINT('Ctrl Pts',(1.66474656556215,4.08569490397205,2.62199192953867));
#10431=CARTESIAN_POINT('Ctrl Pts',(1.62670179878578,4.08960291823166,2.56482472095712));
#10432=CARTESIAN_POINT('Ctrl Pts',(1.58868081506504,4.0935084894609,2.50769324950887));
#10433=CARTESIAN_POINT('Ctrl Pts',(1.54761934451808,4.09741406069015,2.45252647804713));
#10434=CARTESIAN_POINT('Ctrl Pts',(1.50375318288286,4.10131963191939,2.39965957457861));
#10435=CARTESIAN_POINT('Ctrl Pts',(1.4598994066686,4.1052241004275,2.34680759785157));
#10436=CARTESIAN_POINT('Ctrl Pts',(1.41324282530691,4.1091285689356,2.29625457828357));
#10437=CARTESIAN_POINT('Ctrl Pts',(1.36405998580484,4.11303303744371,2.24830320781295));
#10438=CARTESIAN_POINT('Ctrl Pts',(1.31487417413199,4.11693774190295,2.20034893959053));
#10439=CARTESIAN_POINT('Ctrl Pts',(1.26316215513247,4.1208424463622,2.15499697404981));
#10440=CARTESIAN_POINT('Ctrl Pts',(1.20923654449737,4.12474715082145,2.11251239481631));
#10441=CARTESIAN_POINT('Ctrl Pts',(1.15525355468657,4.12865601005466,2.06998261015803));
#10442=CARTESIAN_POINT('Ctrl Pts',(1.09905265975308,4.13256486928788,2.03032660554034));
#10443=CARTESIAN_POINT('Ctrl Pts',(1.04097789456878,4.13647372852109,1.9937678408316));
#10444=CARTESIAN_POINT('Ctrl Pts',(0.982868319018386,4.14038493074821,1.95718716257781));
#10445=CARTESIAN_POINT('Ctrl Pts',(0.922883067278366,4.14429613297533,1.92370765872131));
#10446=CARTESIAN_POINT('Ctrl Pts',(0.861390907329166,4.14820733520245,1.89350687075356));
#10447=CARTESIAN_POINT('Ctrl Pts',(0.799792899752182,4.15212526985656,1.86325409759346));
#10448=CARTESIAN_POINT('Ctrl Pts',(0.736683259057928,4.15604320451067,1.83629149719215));
#10449=CARTESIAN_POINT('Ctrl Pts',(0.672450022014839,4.15996113916478,1.812748189599));
#10450=CARTESIAN_POINT('Ctrl Pts',(0.642655612984952,4.16177846229858,1.80182769160392));
#10451=CARTESIAN_POINT('Ctrl Pts',(0.612619657991374,4.16359578543238,1.79164216046192));
#10452=CARTESIAN_POINT('Ctrl Pts',(0.582381711025327,4.16541310856617,1.78220076717312));
#10453=CARTESIAN_POINT('Ctrl Pts',(0.517182985803051,4.16933160051186,1.76184333988339));
#10454=CARTESIAN_POINT('Ctrl Pts',(0.450786632722353,4.17325009245754,1.74486834658914));
#10455=CARTESIAN_POINT('Ctrl Pts',(0.383576620845942,4.17716858440322,1.73141300283583));
#10456=CARTESIAN_POINT('Ctrl Pts',(0.316467660640327,4.1810811848136,1.71797788947573));
#10457=CARTESIAN_POINT('Ctrl Pts',(0.248547947918729,4.18499378522397,1.70805201884359));
#10458=CARTESIAN_POINT('Ctrl Pts',(0.180216691748753,4.18890638563435,1.70172287625835));
#10459=CARTESIAN_POINT('Ctrl Pts',(0.111965619313498,4.1928143947796,1.69540116064457));
#10460=CARTESIAN_POINT('Ctrl Pts',(0.0433044499019053,4.19672240392485,
1.69266783597897));
#10461=CARTESIAN_POINT('Ctrl Pts',(-0.0253591372019967,4.2006304130701,
1.69355903146726));
#10462=CARTESIAN_POINT('Ctrl Pts',(-0.0939798000670684,4.20453597916911,
1.6944496698351));
#10463=CARTESIAN_POINT('Ctrl Pts',(-0.162602386999179,4.20844154526813,
1.69896032725903));
#10464=CARTESIAN_POINT('Ctrl Pts',(-0.230817406905043,4.21234711136715,
1.70707508100001));
#10465=CARTESIAN_POINT('Ctrl Pts',(-0.29901316643142,4.21625157473709,1.71518754355589));
#10466=CARTESIAN_POINT('Ctrl Pts',(-0.366801099285137,4.22015603810705,
1.72690202420201));
#10467=CARTESIAN_POINT('Ctrl Pts',(-0.433776846712719,4.224060501477,1.7421507444375));
#10468=CARTESIAN_POINT('Ctrl Pts',(-0.500756641560607,4.22796520079809,
1.75740038617044));
#10469=CARTESIAN_POINT('Ctrl Pts',(-0.566923674618833,4.23186990011919,
1.77618457983964));
#10470=CARTESIAN_POINT('Ctrl Pts',(-0.631885572091625,4.23577459944028,
1.79838483505249));
#10471=CARTESIAN_POINT('Ctrl Pts',(-0.696916592506127,4.2396834535708,1.82060871252711));
#10472=CARTESIAN_POINT('Ctrl Pts',(-0.760739452005128,4.24359230770132,
1.84625574620918));
#10473=CARTESIAN_POINT('Ctrl Pts',(-0.822979658704964,4.24750116183183,
1.87515845652983));
#10474=CARTESIAN_POINT('Ctrl Pts',(-0.885257172815169,4.25141235896911,
1.90407849142783));
#10475=CARTESIAN_POINT('Ctrl Pts',(-0.945949711592307,4.25532355610639,
1.93625785640227));
#10476=CARTESIAN_POINT('Ctrl Pts',(-1.00470790265019,4.25923475324366,1.97148336373439));
#10477=CARTESIAN_POINT('Ctrl Pts',(-1.06356723653612,4.26315268288125,2.00676950614337));
#10478=CARTESIAN_POINT('Ctrl Pts',(-1.12048516969907,4.26707061251884,2.04511198123528));
#10479=CARTESIAN_POINT('Ctrl Pts',(-1.17514251896323,4.27098854215643,2.08625512148463));
#10480=CARTESIAN_POINT('Ctrl Pts',(-1.20049585121116,4.27280591115004,2.10533975911357));
#10481=CARTESIAN_POINT('Ctrl Pts',(-1.22536326940057,4.27462328014365,2.12502645043354));
#10482=CARTESIAN_POINT('Ctrl Pts',(-1.24971558638332,4.27644064913727,2.14528696442451));
#10483=CARTESIAN_POINT('Ctrl Pts',(-1.30222242483607,4.2803591387095,2.18897133071489));
#10484=CARTESIAN_POINT('Ctrl Pts',(-1.3525398362606,4.28427762828174,2.23549850288803));
#10485=CARTESIAN_POINT('Ctrl Pts',(-1.40034404905102,4.28819611785397,2.28462062633965));
#10486=CARTESIAN_POINT('Ctrl Pts',(-1.44807638643017,4.29210871583145,2.33366889285233));
#10487=CARTESIAN_POINT('Ctrl Pts',(-1.49330268437293,4.29602131380893,2.38530401766588));
#10488=CARTESIAN_POINT('Ctrl Pts',(-1.53573264762283,4.2999339117864,2.43923833804847));
#10489=CARTESIAN_POINT('Ctrl Pts',(-1.57811282031323,4.30384191842259,2.49310936778025));
#10490=CARTESIAN_POINT('Ctrl Pts',(-1.6177028727059,4.30774992505877,2.54927384999246));
#10491=CARTESIAN_POINT('Ctrl Pts',(-1.65425102822595,4.31165793169495,2.60740911472673));
#10492=CARTESIAN_POINT('Ctrl Pts',(-1.69077633565019,4.31556349523904,2.66550803617417));
#10493=CARTESIAN_POINT('Ctrl Pts',(-1.72426325734885,4.31946905878312,2.72557488075027));
#10494=CARTESIAN_POINT('Ctrl Pts',(-1.75450273635882,4.3233746223272,2.78725718382899));
#10495=CARTESIAN_POINT('Ctrl Pts',(-1.7847336769792,4.32727908310019,2.84892207035321));
#10496=CARTESIAN_POINT('Ctrl Pts',(-1.8117187788626,4.33118354387319,2.91220106849711));
#10497=CARTESIAN_POINT('Ctrl Pts',(-1.83529531184882,4.33508800464618,2.97671785596931));
#10498=CARTESIAN_POINT('Ctrl Pts',(-1.85887326936181,4.3389927013321,3.04123854163511));
#10499=CARTESIAN_POINT('Ctrl Pts',(-1.87904208272449,4.34289739801802,3.10699670233851));
#10500=CARTESIAN_POINT('Ctrl Pts',(-1.89568811035567,4.34680209470394,3.17359853303731));
#10501=CARTESIAN_POINT('Ctrl Pts',(-1.91235185009414,4.35071094615929,3.24027123102034));
#10502=CARTESIAN_POINT('Ctrl Pts',(-1.92548520407721,4.35461979761464,3.30778891251314));
#10503=CARTESIAN_POINT('Ctrl Pts',(-1.93502537597305,4.35852864906998,3.37574617666332));
#10504=CARTESIAN_POINT('Ctrl Pts',(-1.94457126628318,4.36243984350533,3.44374417464873));
#10505=CARTESIAN_POINT('Ctrl Pts',(-1.95051964551699,4.36635103794068,3.51218178970454));
#10506=CARTESIAN_POINT('Ctrl Pts',(-1.95285973907249,4.37026223237603,3.58064988416092));
#10507=CARTESIAN_POINT('Ctrl Pts',(-1.95520386071968,4.37418015929856,3.64923583534251));
#10508=CARTESIAN_POINT('Ctrl Pts',(-1.95392730970642,4.37809808622109,3.71785187923863));
#10509=CARTESIAN_POINT('Ctrl Pts',(-1.94907137633539,4.38201601314361,3.7860911515538));
#10510=CARTESIAN_POINT('Ctrl Pts',(-1.94681887506376,4.38383340533185,3.81774501414217));
#10511=CARTESIAN_POINT('Ctrl Pts',(-1.9437969214201,4.3856507975201,3.8493179137455));
#10512=CARTESIAN_POINT('Ctrl Pts',(-1.94001336524288,4.38746818970834,3.8807700083025));
#10513=CARTESIAN_POINT('Ctrl Pts',(-1.93185561275431,4.39138668198172,3.94858409394713));
#10514=CARTESIAN_POINT('Ctrl Pts',(-1.92012173726112,4.39530517425511,4.01610403779491));
#10515=CARTESIAN_POINT('Ctrl Pts',(-1.90484397768049,4.39922366652849,4.08292336594094));
#10516=CARTESIAN_POINT('Ctrl Pts',(-1.88958918859449,4.40313626725048,4.14964222955151));
#10517=CARTESIAN_POINT('Ctrl Pts',(-1.8708011990718,4.40704886797247,4.2156620925364));
#10518=CARTESIAN_POINT('Ctrl Pts',(-1.84856385522709,4.41096146869446,4.28058296561144));
#10519=CARTESIAN_POINT('Ctrl Pts',(-1.82635260607385,4.41486947812581,4.34542765646958));
#10520=CARTESIAN_POINT('Ctrl Pts',(-1.80070020003047,4.41877748755716,4.40917545560964));
#10521=CARTESIAN_POINT('Ctrl Pts',(-1.77174079835073,4.42268549698851,4.47143969972419));
#10522=CARTESIAN_POINT('Ctrl Pts',(-1.74279950042004,4.42659106335758,4.53366501982148));
#10523=CARTESIAN_POINT('Ctrl Pts',(-1.71055551477642,4.43049662972664,4.59440817974515));
#10524=CARTESIAN_POINT('Ctrl Pts',(-1.67519122308986,4.4344021960957,4.65330220067422));
#10525=CARTESIAN_POINT('Ctrl Pts',(-1.63983691659179,4.43830665971919,4.71217959274204));
#10526=CARTESIAN_POINT('Ctrl Pts',(-1.60136430610727,4.44221112334267,4.76920846090665));
#10527=CARTESIAN_POINT('Ctrl Pts',(-1.56000096824237,4.44611558696615,4.82404776432433));
#10528=CARTESIAN_POINT('Ctrl Pts',(-1.51863513092428,4.45002028652379,4.87889038150437));
#10529=CARTESIAN_POINT('Ctrl Pts',(-1.47437851761472,4.45392498608142,4.93154278020573));
#10530=CARTESIAN_POINT('Ctrl Pts',(-1.42750004749011,4.45782968563906,4.98169563909042));
#10531=CARTESIAN_POINT('Ctrl Pts',(-1.38057169649302,4.46173853997863,5.03190186294952));
#10532=CARTESIAN_POINT('Ctrl Pts',(-1.33101625765954,4.4656473943182,5.07960287931863));
#10533=CARTESIAN_POINT('Ctrl Pts',(-1.27914000413541,4.46955624865777,5.12452575893493));
#10534=CARTESIAN_POINT('Ctrl Pts',(-1.22723265566561,4.47346744598868,5.16947556560178));
#10535=CARTESIAN_POINT('Ctrl Pts',(-1.17300211219332,4.4773786433196,5.21164361948927));
#10536=CARTESIAN_POINT('Ctrl Pts',(-1.11678604131831,4.48128984065052,5.25079864001244));
#10537=CARTESIAN_POINT('Ctrl Pts',(-1.0604732038458,4.48520777045584,5.29002105937819));
#10538=CARTESIAN_POINT('Ctrl Pts',(-1.00216843533805,4.48912570026116,5.32621983501009));
#10539=CARTESIAN_POINT('Ctrl Pts',(-0.942235775033817,4.49304363006647,
5.35920863584016));
#10540=CARTESIAN_POINT('Ctrl Pts',(-0.914435475194858,4.49486099680412,
5.37451078578224));
#10541=CARTESIAN_POINT('Ctrl Pts',(-0.886285215289913,4.49667836354177,
5.3891229312105));
#10542=CARTESIAN_POINT('Ctrl Pts',(-0.857822709676755,4.49849573027942,
5.40303002236759));
#10543=CARTESIAN_POINT('Ctrl Pts',(-0.79645365023014,4.50241422181615,5.43301561518744));
#10544=CARTESIAN_POINT('Ctrl Pts',(-0.733389092946571,4.50633271335287,
5.45983885890344));
#10545=CARTESIAN_POINT('Ctrl Pts',(-0.668987832150792,4.51025120488959,
5.48330603489981));
#10546=CARTESIAN_POINT('Ctrl Pts',(-0.604683400411588,4.51416380486715,
5.50673792735539));
#10547=CARTESIAN_POINT('Ctrl Pts',(-0.539046712223257,4.5180764048447,5.52682359956585));
#10548=CARTESIAN_POINT('Ctrl Pts',(-0.472459149121543,4.52198900482225,
5.54341618556755));
#10549=CARTESIAN_POINT('Ctrl Pts',(-0.405949724182622,4.52589701350138,
5.55998930075329));
#10550=CARTESIAN_POINT('Ctrl Pts',(-0.338492115304038,4.5298050221805,5.57307735214724));
#10551=CARTESIAN_POINT('Ctrl Pts',(-0.270483845284502,4.53371303085962,
5.58258295766678));
#10552=CARTESIAN_POINT('Ctrl Pts',(-0.202518090200716,4.53761859647207,
5.59208262081773));
#10553=CARTESIAN_POINT('Ctrl Pts',(-0.134002842795731,4.54152416208452,
5.59800421276478));
#10554=CARTESIAN_POINT('Ctrl Pts',(-0.0653452906021543,4.54542972769697,
5.60030153033166));
#10555=CARTESIAN_POINT('Ctrl Pts',(0.00329287591453474,4.54933419056063,
5.60259819924366));
#10556=CARTESIAN_POINT('Ctrl Pts',(0.0720727761918795,4.55323865342428,
5.60127260884809));
#10557=CARTESIAN_POINT('Ctrl Pts',(0.14058445188283,4.55714311628793,5.59633059137483));
#10558=CARTESIAN_POINT('Ctrl Pts',(0.209100267478285,4.56104781508368,5.59138827527392));
#10559=CARTESIAN_POINT('Ctrl Pts',(0.277347336006442,4.56495251387944,5.5828291361928));
#10560=CARTESIAN_POINT('Ctrl Pts',(0.344919875101767,4.56885721267519,5.5707109476392));
#10561=CARTESIAN_POINT('Ctrl Pts',(0.412564314572669,4.57276606625503,5.55857986476019));
#10562=CARTESIAN_POINT('Ctrl Pts',(0.47953230729278,4.57667491983486,5.54288226179697));
#10563=CARTESIAN_POINT('Ctrl Pts',(0.545428336570195,4.5805837734147,5.52372704266035));
#10564=CARTESIAN_POINT('Ctrl Pts',(0.61136386434293,4.58449496998601,5.50456034176464));
#10565=CARTESIAN_POINT('Ctrl Pts',(0.676225685518648,4.58840616655732,5.48193206200186));
#10566=CARTESIAN_POINT('Ctrl Pts',(0.739636199691951,4.59231736312863,5.45600008922649));
#10567=CARTESIAN_POINT('Ctrl Pts',(0.803155864651577,4.5962352921825,5.43002347881877));
#10568=CARTESIAN_POINT('Ctrl Pts',(0.865218792240826,4.60015322123638,5.40073203547596));
#10569=CARTESIAN_POINT('Ctrl Pts',(0.925470798061767,4.60407115029026,5.36833020268388));
#10570=CARTESIAN_POINT('Ctrl Pts',(0.953419338835436,4.60588852381034,5.35330026413508));
#10571=CARTESIAN_POINT('Ctrl Pts',(0.980978626059207,4.60770589733042,5.33760169347744));
#10572=CARTESIAN_POINT('Ctrl Pts',(1.00811553775735,4.6095232708505,5.32125798199465));
#10573=CARTESIAN_POINT('Ctrl Pts',(1.06662620765758,4.6134417617717,5.28601883915663));
#10574=CARTESIAN_POINT('Ctrl Pts',(1.12340266514511,4.61736025269291,5.2476384125661));
#10575=CARTESIAN_POINT('Ctrl Pts',(1.17808737194234,4.62127874361412,5.20631272915261));
#10576=CARTESIAN_POINT('Ctrl Pts',(1.23268985867502,4.62519134296901,5.1650491801192));
#10577=CARTESIAN_POINT('Ctrl Pts',(1.28520644730769,4.6291039423239,5.12084945702431));
#10578=CARTESIAN_POINT('Ctrl Pts',(1.33530666907632,4.63301654167879,5.07395400069754));
#10579=CARTESIAN_POINT('Ctrl Pts',(1.38534809989083,4.63692454972768,5.02711357463857));
#10580=CARTESIAN_POINT('Ctrl Pts',(1.43297843794734,4.64083255777657,4.97758403233599));
#10581=CARTESIAN_POINT('Ctrl Pts',(1.4778999945136,4.64474056582545,4.9256462456019));
#10582=CARTESIAN_POINT('Ctrl Pts',(1.52279346860112,4.64864613080332,4.87374092750655));
#10583=CARTESIAN_POINT('Ctrl Pts',(1.56498119938352,4.65255169578119,4.81943072256503));
#10584=CARTESIAN_POINT('Ctrl Pts',(1.60420321923423,4.65645726075905,4.76303241645457));
#10585=CARTESIAN_POINT('Ctrl Pts',(1.64341416458766,4.66036172298472,4.70665003463588));
#10586=CARTESIAN_POINT('Ctrl Pts',(1.6796607807379,4.66426618521039,4.64818112563726));
#10587=CARTESIAN_POINT('Ctrl Pts',(1.71272528491316,4.66817064743605,4.58797306596677));
#10588=CARTESIAN_POINT('Ctrl Pts',(1.74579178703228,4.67207534559135,4.52776136818568));
#10589=CARTESIAN_POINT('Ctrl Pts',(1.77567556097397,4.67598004374665,4.46581074337491));
#10590=CARTESIAN_POINT('Ctrl Pts',(1.80220470312597,4.67988474190195,4.40249327508376));
#10591=CARTESIAN_POINT('Ctrl Pts',(1.82876207354774,4.68379359484191,4.33910843399309));
#10592=CARTESIAN_POINT('Ctrl Pts',(1.85195749827294,4.68770244778187,4.27435430137876));
#10593=CARTESIAN_POINT('Ctrl Pts',(1.87166757980066,4.69161130072183,4.20862211436267));
#10594=CARTESIAN_POINT('Ctrl Pts',(1.89138947567435,4.69552249665266,4.14285052706313));
#10595=CARTESIAN_POINT('Ctrl Pts',(1.90762175436047,4.69943369258349,4.07610019650604));
#10596=CARTESIAN_POINT('Ctrl Pts',(1.92029187621526,4.70334488851431,4.00877392279351));
#10597=CARTESIAN_POINT('Ctrl Pts',(1.93298380762609,4.70726281693342,3.94133175784042));
#10598=CARTESIAN_POINT('Ctrl Pts',(1.94210127926275,4.71118074535253,3.87331215822697));
#10599=CARTESIAN_POINT('Ctrl Pts',(1.94762356115872,4.71509867377163,3.80512355253726));
#10600=CARTESIAN_POINT('Ctrl Pts',(1.95018513944006,4.71691605298828,3.77349343030518));
#10601=CARTESIAN_POINT('Ctrl Pts',(1.951973883556,4.71873343220493,3.74182694727277));
#10602=CARTESIAN_POINT('Ctrl Pts',(1.95299152617942,4.72055081142158,3.71016467356757));
#10603=CARTESIAN_POINT('Ctrl Pts',(1.95365963993518,4.72174397690631,3.68937741474616));
#10604=CARTESIAN_POINT('Ctrl Pts',(1.95399588157958,4.72293714239104,3.66857943228896));
#10605=CARTESIAN_POINT('Ctrl Pts',(1.95399996239942,4.72413030787577,3.64777779982394));
#10606=CARTESIAN_POINT('Origin',(0.,0.,3.64739446828387));
#10607=CARTESIAN_POINT('',(1.95399938884984,5.5258696920781,3.64893990493632));
#10608=CARTESIAN_POINT('',(1.95399943981962,5.42413030787577,3.64887405762317));
#10609=CARTESIAN_POINT('',(1.954,4.33875158023511E-16,3.64739446828387));
#10610=CARTESIAN_POINT('Ctrl Pts',(1.95399938884984,5.5258696920781,3.64893990493632));
#10611=CARTESIAN_POINT('Ctrl Pts',(1.9539356881594,5.5212902068915,3.72948096754413));
#10612=CARTESIAN_POINT('Ctrl Pts',(1.94888837279949,5.51671072170489,3.80981306186041));
#10613=CARTESIAN_POINT('Ctrl Pts',(1.9389580842007,5.51213123651829,3.88938113674468));
#10614=CARTESIAN_POINT('Ctrl Pts',(1.92891637635983,5.50750036886043,3.96984197667887));
#10615=CARTESIAN_POINT('Ctrl Pts',(1.91388160449032,5.50286950120256,4.04952144814088));
#10616=CARTESIAN_POINT('Ctrl Pts',(1.89400709304294,5.4982386335447,4.12786624841569));
#10617=CARTESIAN_POINT('Ctrl Pts',(1.88182705946909,5.49540062045954,4.17587961972344));
#10618=CARTESIAN_POINT('Ctrl Pts',(1.8678302625667,5.49256260737438,4.22339212396168));
#10619=CARTESIAN_POINT('Ctrl Pts',(1.85206076918552,5.48972459428922,4.27028041871456));
#10620=CARTESIAN_POINT('Ctrl Pts',(1.83028813032353,5.48580620372998,4.33501819334256));
#10621=CARTESIAN_POINT('Ctrl Pts',(1.80507401469036,5.48188781317074,4.39874111135267));
#10622=CARTESIAN_POINT('Ctrl Pts',(1.77653259424178,5.47796942261151,4.4610577534311));
#10623=CARTESIAN_POINT('Ctrl Pts',(1.74803409982399,5.47405692527522,4.52328067185963));
#10624=CARTESIAN_POINT('Ctrl Pts',(1.71621843544014,5.47014442793892,4.58410106841738));
#10625=CARTESIAN_POINT('Ctrl Pts',(1.68124898529418,5.46623193060263,4.64314436130283));
#10626=CARTESIAN_POINT('Ctrl Pts',(1.64632058913066,5.4623240265212,4.70211833761915));
#10627=CARTESIAN_POINT('Ctrl Pts',(1.60824600996504,5.45841612243977,4.75931893258246));
#10628=CARTESIAN_POINT('Ctrl Pts',(1.56723518853597,5.45450821835834,4.81439483838433));
#10629=CARTESIAN_POINT('Ctrl Pts',(1.52625001755183,5.45060275849711,4.86943629665652));
#10630=CARTESIAN_POINT('Ctrl Pts',(1.48233254040991,5.44669729863589,4.92235530833293));
#10631=CARTESIAN_POINT('Ctrl Pts',(1.43573591095886,5.44279183877466,4.97282963983438));
#10632=CARTESIAN_POINT('Ctrl Pts',(1.3891524504077,5.43888748265443,5.02328970653972));
#10633=CARTESIAN_POINT('Ctrl Pts',(1.33989167411641,5.43498312653419,5.07130610346387));
#10634=CARTESIAN_POINT('Ctrl Pts',(1.2882457154627,5.43107877041396,5.11659117961697));
#10635=CARTESIAN_POINT('Ctrl Pts',(1.23659664695655,5.4271741791936,5.16187898260307));
#10636=CARTESIAN_POINT('Ctrl Pts',(1.18256248241879,5.42326958797323,5.20443481600125));
#10637=CARTESIAN_POINT('Ctrl Pts',(1.12646938739104,5.41936499675287,5.24401048952093));
#10638=CARTESIAN_POINT('Ctrl Pts',(1.07031661254359,5.41545625127252,5.28362826927595));
#10639=CARTESIAN_POINT('Ctrl Pts',(1.01210093814373,5.41154750579218,5.3202592773975));
#10640=CARTESIAN_POINT('Ctrl Pts',(0.952177706509464,5.40763876031183,5.35369854881183));
#10641=CARTESIAN_POINT('Ctrl Pts',(0.892218562522306,5.40372767229682,5.38715786058251));
#10642=CARTESIAN_POINT('Ctrl Pts',(0.830550266194682,5.39981658428181,5.41742141207676));
#10643=CARTESIAN_POINT('Ctrl Pts',(0.767550432646793,5.39590549626681,5.44433139910357));
#10644=CARTESIAN_POINT('Ctrl Pts',(0.704442145284472,5.39198767533855,5.47128771150261));
#10645=CARTESIAN_POINT('Ctrl Pts',(0.639998207402256,5.3880698544103,5.49487876839399));
#10646=CARTESIAN_POINT('Ctrl Pts',(0.574612917820234,5.38415203348204,5.51499613745054));
#10647=CARTESIAN_POINT('Ctrl Pts',(0.544266505187708,5.38233370689407,5.52433294679058));
#10648=CARTESIAN_POINT('Ctrl Pts',(0.51371748425252,5.3805153803061,5.53292222715602));
#10649=CARTESIAN_POINT('Ctrl Pts',(0.483005906313117,5.37869705371813,5.54075689911074));
#10650=CARTESIAN_POINT('Ctrl Pts',(0.416821913118872,5.3747785277876,5.55764075562745));
#10651=CARTESIAN_POINT('Ctrl Pts',(0.349620703532056,5.37086000185707,5.57108354879797));
#10652=CARTESIAN_POINT('Ctrl Pts',(0.281792968696771,5.36694147592654,5.5809685482697));
#10653=CARTESIAN_POINT('Ctrl Pts',(0.214067207838018,5.36302884120956,5.59083868637673));
#10654=CARTESIAN_POINT('Ctrl Pts',(0.145717273873277,5.35911620649259,5.59716157616641));
#10655=CARTESIAN_POINT('Ctrl Pts',(0.0771464480080062,5.35520357177562,
5.5998709535609));
#10656=CARTESIAN_POINT('Ctrl Pts',(0.00865608095150007,5.35129552801879,
5.60257715185882));
#10657=CARTESIAN_POINT('Ctrl Pts',(-0.0600541741936425,5.34738748426196,
5.60167823916572));
#10658=CARTESIAN_POINT('Ctrl Pts',(-0.128575292284244,5.34347944050513,
5.59715968343518));
#10659=CARTESIAN_POINT('Ctrl Pts',(-0.19705357853462,5.33957383962592,5.59264395220695));
#10660=CARTESIAN_POINT('Ctrl Pts',(-0.265342472663803,5.33566823874671,
5.58451309856255));
#10661=CARTESIAN_POINT('Ctrl Pts',(-0.333033891360969,5.3317626378675,5.572804665412));
#10662=CARTESIAN_POINT('Ctrl Pts',(-0.400706199678621,5.32785813960242,
5.56109953774101));
#10663=CARTESIAN_POINT('Ctrl Pts',(-0.467780883087573,5.32395364133734,
5.54581891941343));
#10664=CARTESIAN_POINT('Ctrl Pts',(-0.533857724051586,5.32004914307227,
5.52705186538326));
#10665=CARTESIAN_POINT('Ctrl Pts',(-0.599938559117321,5.31614440879465,
5.50828367695379));
#10666=CARTESIAN_POINT('Ctrl Pts',(-0.665020959650626,5.31223967451703,
5.48602877125568));
#10667=CARTESIAN_POINT('Ctrl Pts',(-0.728719356347817,5.30833494023941,
5.46042621088631));
#10668=CARTESIAN_POINT('Ctrl Pts',(-0.792485528538388,5.30442605130004,
5.43479640923221));
#10669=CARTESIAN_POINT('Ctrl Pts',(-0.85486430094833,5.30051716236068,5.40581202823352));
#10670=CARTESIAN_POINT('Ctrl Pts',(-0.915490550093738,5.29660827342131,
5.37366010621132));
#10671=CARTESIAN_POINT('Ctrl Pts',(-0.976153138378129,5.29269704150905,
5.34148891245156));
#10672=CARTESIAN_POINT('Ctrl Pts',(-1.03506069105742,5.28878580959679,5.30614665209339));
#10673=CARTESIAN_POINT('Ctrl Pts',(-1.09187558439369,5.28487457768452,5.26786468035349));
#10674=CARTESIAN_POINT('Ctrl Pts',(-1.14878826855107,5.28095661368921,5.22951681699203));
#10675=CARTESIAN_POINT('Ctrl Pts',(-1.2036007120852,5.27703864969391,5.18821943943032));
#10676=CARTESIAN_POINT('Ctrl Pts',(-1.25600768300803,5.2731206856986,5.14424472807101));
#10677=CARTESIAN_POINT('Ctrl Pts',(-1.28031277631211,5.27130362818142,5.1238503140496));
#10678=CARTESIAN_POINT('Ctrl Pts',(-1.30410099538044,5.26948657066424,5.10288056396188));
#10679=CARTESIAN_POINT('Ctrl Pts',(-1.32734469991678,5.26766951314705,5.08136519588009));
#10680=CARTESIAN_POINT('Ctrl Pts',(-1.37746993607036,5.26375101396759,5.03496713121941));
#10681=CARTESIAN_POINT('Ctrl Pts',(-1.42525856221547,5.25983251478813,4.98584591761483));
#10682=CARTESIAN_POINT('Ctrl Pts',(-1.4704003566331,5.25591401560867,4.93426617564761));
#10683=CARTESIAN_POINT('Ctrl Pts',(-1.51547428213325,5.25200140773904,4.88276398179951));
#10684=CARTESIAN_POINT('Ctrl Pts',(-1.55790895241811,5.24808879986942,4.82881096259533));
#10685=CARTESIAN_POINT('Ctrl Pts',(-1.59742967920943,5.24417619199979,4.7727097218821));
#10686=CARTESIAN_POINT('Ctrl Pts',(-1.63690403325636,5.24026817509747,4.71667430912061));
#10687=CARTESIAN_POINT('Ctrl Pts',(-1.67347095248102,5.23636015819515,4.65849608111685));
#10688=CARTESIAN_POINT('Ctrl Pts',(-1.70689606355721,5.23245214129283,4.59851056435885));
#10689=CARTESIAN_POINT('Ctrl Pts',(-1.74030028090185,5.22854656725617,4.53856254399932));
#10690=CARTESIAN_POINT('Ctrl Pts',(-1.77056634709308,5.22464099321951,4.47680990453237));
#10691=CARTESIAN_POINT('Ctrl Pts',(-1.79750412333859,5.22073541918285,4.41361566779532));
#10692=CARTESIAN_POINT('Ctrl Pts',(-1.82443429493401,5.21683094770654,4.3504392710631));
#10693=CARTESIAN_POINT('Ctrl Pts',(-1.84803784911865,5.21292647623023,4.28582253714577));
#10694=CARTESIAN_POINT('Ctrl Pts',(-1.86817217000141,5.20902200475392,4.22014986392169));
#10695=CARTESIAN_POINT('Ctrl Pts',(-1.88830770843132,5.20511729716942,4.15447321939029));
#10696=CARTESIAN_POINT('Ctrl Pts',(-1.90497345537371,5.20121258958491,4.08774097969491));
#10697=CARTESIAN_POINT('Ctrl Pts',(-1.91807673883904,5.19730788200041,4.02035240683005));
#10698=CARTESIAN_POINT('Ctrl Pts',(-1.93119396548151,5.19339901942455,3.95289212592253));
#10699=CARTESIAN_POINT('Ctrl Pts',(-1.94074106941275,5.18949015684868,3.8847746017087));
#10700=CARTESIAN_POINT('Ctrl Pts',(-1.94667676563993,5.18558129427282,3.81640798880124));
#10701=CARTESIAN_POINT('Ctrl Pts',(-1.95261601995247,5.18167008857389,3.7480003943078));
#10702=CARTESIAN_POINT('Ctrl Pts',(-1.95493954153139,5.17775888287496,3.67934390549862));
#10703=CARTESIAN_POINT('Ctrl Pts',(-1.95365819189621,5.17384767717603,3.6108476594378));
#10704=CARTESIAN_POINT('Ctrl Pts',(-1.95237463659777,5.16992973888634,3.54223350671894));
#10705=CARTESIAN_POINT('Ctrl Pts',(-1.94747386063335,5.16601180059666,3.4737806374872));
#10706=CARTESIAN_POINT('Ctrl Pts',(-1.93901859753382,5.16209386230697,3.40589316721499));
#10707=CARTESIAN_POINT('Ctrl Pts',(-1.93509670812356,5.16027656572998,3.37440424160542));
#10708=CARTESIAN_POINT('Ctrl Pts',(-1.93041080123305,5.15845926915298,3.34303681436157));
#10709=CARTESIAN_POINT('Ctrl Pts',(-1.92497081948355,5.15664197257598,3.31183025067891));
#10710=CARTESIAN_POINT('Ctrl Pts',(-1.91324106259502,5.15272349490011,3.24454226660473));
#10711=CARTESIAN_POINT('Ctrl Pts',(-1.89795575006275,5.14880501722424,3.17773696910645));
#10712=CARTESIAN_POINT('Ctrl Pts',(-1.87916855139228,5.14488653954837,3.11181855820364));
#10713=CARTESIAN_POINT('Ctrl Pts',(-1.86040960103854,5.14097395367151,3.04599926181934));
#10714=CARTESIAN_POINT('Ctrl Pts',(-1.83815934832929,5.13706136779465,2.98106467459702));
#10715=CARTESIAN_POINT('Ctrl Pts',(-1.81252265527332,5.13314878191779,2.91740979438929));
#10716=CARTESIAN_POINT('Ctrl Pts',(-1.78691604795421,5.12924078762491,2.85382961585903));
#10717=CARTESIAN_POINT('Ctrl Pts',(-1.75793107587758,5.12533279333203,2.7915266157593));
#10718=CARTESIAN_POINT('Ctrl Pts',(-1.72572214182345,5.12142479903915,2.7308798261639));
#10719=CARTESIAN_POINT('Ctrl Pts',(-1.69353334444491,5.11751924798183,2.67027095228239));
#10720=CARTESIAN_POINT('Ctrl Pts',(-1.65812481356218,5.11361369692452,2.61131666823852));
#10721=CARTESIAN_POINT('Ctrl Pts',(-1.61969806496519,5.10970814586721,2.55437380134841));
#10722=CARTESIAN_POINT('Ctrl Pts',(-1.58128216776611,5.10580369770541,2.4974470146558));
#10723=CARTESIAN_POINT('Ctrl Pts',(-1.53985001983799,5.10189924954361,2.44253092495088));
#10724=CARTESIAN_POINT('Ctrl Pts',(-1.49564689828911,5.09799480138181,2.3899540698402));
#10725=CARTESIAN_POINT('Ctrl Pts',(-1.45144110711249,5.09409011741261,2.3373740393739));
#10726=CARTESIAN_POINT('Ctrl Pts',(-1.40446432849758,5.09018543344342,2.28713389874032));
#10727=CARTESIAN_POINT('Ctrl Pts',(-1.35500144837191,5.08628074947422,2.23952832588608));
#10728=CARTESIAN_POINT('Ctrl Pts',(-1.30548593831245,5.08237191080844,2.19187209932667));
#10729=CARTESIAN_POINT('Ctrl Pts',(-1.25347940263471,5.07846307214267,2.14685637657934));
#10730=CARTESIAN_POINT('Ctrl Pts',(-1.1993021061283,5.07455423347689,2.10473752060035));
#10731=CARTESIAN_POINT('Ctrl Pts',(-1.14509233627885,5.07064305189135,2.06259341898994));
#10732=CARTESIAN_POINT('Ctrl Pts',(-1.08870961977551,5.06673187030581,2.02334992078389));
#10733=CARTESIAN_POINT('Ctrl Pts',(-1.03050337127767,5.06282068872027,1.98722013955048));
#10734=CARTESIAN_POINT('Ctrl Pts',(-0.972196929213085,5.05890277460612,
1.95102816616862));
#10735=CARTESIAN_POINT('Ctrl Pts',(-0.912061121091908,5.05498486049197,
1.91796084372819));
#10736=CARTESIAN_POINT('Ctrl Pts',(-0.850469321204268,5.05106694637782,
1.88818500557332));
#10737=CARTESIAN_POINT('Ctrl Pts',(-0.821897129951727,5.04924944158685,
1.87437211255805));
#10738=CARTESIAN_POINT('Ctrl Pts',(-0.793011879616013,5.04743193679587,
1.8612668600447));
#10739=CARTESIAN_POINT('Ctrl Pts',(-0.7638520361295,5.0456144320049,1.84888228681252));
#10740=CARTESIAN_POINT('Ctrl Pts',(-0.700984107837436,5.04169593494841,
1.82218144178747));
#10741=CARTESIAN_POINT('Ctrl Pts',(-0.636590155551062,5.03777743789193,
1.79872813327963));
#10742=CARTESIAN_POINT('Ctrl Pts',(-0.571038710239946,5.03385894083544,
1.77869684924341));
#10743=CARTESIAN_POINT('Ctrl Pts',(-0.505585822135277,5.02994633527565,
1.75869568242865));
#10744=CARTESIAN_POINT('Ctrl Pts',(-0.438979361448358,5.02603372971586,
1.74210647146396));
#10745=CARTESIAN_POINT('Ctrl Pts',(-0.37160793886445,5.02212112415607,1.72905572349115));
#10746=CARTESIAN_POINT('Ctrl Pts',(-0.30431557304831,5.01821310983003,1.71602028987437));
#10747=CARTESIAN_POINT('Ctrl Pts',(-0.236260508593127,5.01430509550399,
1.70651516594548));
#10748=CARTESIAN_POINT('Ctrl Pts',(-0.167844859934866,5.01039708117795,
1.70061659112545));
#10749=CARTESIAN_POINT('Ctrl Pts',(-0.099471980176605,5.00649150988179,
1.69472170370094));
#10750=CARTESIAN_POINT('Ctrl Pts',(-0.0307394522219087,5.00258593858563,
1.69242893512387));
#10751=CARTESIAN_POINT('Ctrl Pts',(0.0379436627796952,4.99868036728946,
1.69376290669022));
#10752=CARTESIAN_POINT('Ctrl Pts',(0.106607385407991,4.99477589871406,1.6950965016156));
#10753=CARTESIAN_POINT('Ctrl Pts',(0.175221231337193,4.99087143013866,1.70005479430132));
#10754=CARTESIAN_POINT('Ctrl Pts',(0.243376122230749,4.98696696156325,1.70861029692082));
#10755=CARTESIAN_POINT('Ctrl Pts',(0.311535131800966,4.98306225703642,1.71716631655895));
#10756=CARTESIAN_POINT('Ctrl Pts',(0.379234643660844,4.97915755250959,1.72931991390676));
#10757=CARTESIAN_POINT('Ctrl Pts',(0.44607249438087,4.97525284798276,1.74499195310554));
#10758=CARTESIAN_POINT('Ctrl Pts',(0.512981463455144,4.971343988682,1.76068066802959));
#10759=CARTESIAN_POINT('Ctrl Pts',(0.57902646198267,4.96743512938124,1.7798951836522));
#10760=CARTESIAN_POINT('Ctrl Pts',(0.643818279759381,4.96352627008048,1.802505847622));
#10761=CARTESIAN_POINT('Ctrl Pts',(0.708648934144848,4.95961506778574,1.82513006456099));
#10762=CARTESIAN_POINT('Ctrl Pts',(0.772224457656997,4.95570386549099,1.85115429490052));
#10763=CARTESIAN_POINT('Ctrl Pts',(0.834176119683657,4.95179266319625,1.88040091952668));
#10764=CARTESIAN_POINT('Ctrl Pts',(0.89623442027662,4.9478747284751,1.90969788692037));
#10765=CARTESIAN_POINT('Ctrl Pts',(0.956662847974734,4.94395679375395,1.94222808592337));
#10766=CARTESIAN_POINT('Ctrl Pts',(1.01511851568101,4.9400388590328,1.9777686422014));
#10767=CARTESIAN_POINT('Ctrl Pts',(1.04223300575413,4.93822153649981,1.9942540250258));
#10768=CARTESIAN_POINT('Ctrl Pts',(1.06892347732324,4.93640421396681,2.01138649999389));
#10769=CARTESIAN_POINT('Ctrl Pts',(1.09515809873353,4.93458689143382,2.02914086060109));
#10770=CARTESIAN_POINT('Ctrl Pts',(1.15152628047914,4.93068215939184,2.06728820070681));
#10771=CARTESIAN_POINT('Ctrl Pts',(1.20601427441916,4.92677742734985,2.10846238665927));
#10772=CARTESIAN_POINT('Ctrl Pts',(1.25827678983222,4.92287269530786,2.15245115157601));
#10773=CARTESIAN_POINT('Ctrl Pts',(1.3123737685588,4.91883090350855,2.19798396340301));
#10774=CARTESIAN_POINT('Ctrl Pts',(1.36408562775225,4.91478911170923,2.24653241326189));
#10775=CARTESIAN_POINT('Ctrl Pts',(1.41306090869165,4.91074731990991,2.29781124805345));
#10776=CARTESIAN_POINT('Ctrl Pts',(1.46024774346122,4.90685312352861,2.34721751705432));
#10777=CARTESIAN_POINT('Ctrl Pts',(1.50489402519352,4.90295892714731,2.39915781793867));
#10778=CARTESIAN_POINT('Ctrl Pts',(1.54671985078529,4.89906473076601,2.45333680502522));
#10779=CARTESIAN_POINT('Ctrl Pts',(1.58852053660532,4.89517287502489,2.50748322736618));
#10780=CARTESIAN_POINT('Ctrl Pts',(1.62750382633125,4.89128101928378,2.56386527560244));
#10781=CARTESIAN_POINT('Ctrl Pts',(1.66342951017411,4.88738916354266,2.62215387960144));
#10782=CARTESIAN_POINT('Ctrl Pts',(1.69934614678611,4.88349828789472,2.68042780467435));
#10783=CARTESIAN_POINT('Ctrl Pts',(1.73220644619769,4.87960741224677,2.74060691051942));
#10784=CARTESIAN_POINT('Ctrl Pts',(1.7618140741169,4.87571653659883,2.80233401586428));
#10785=CARTESIAN_POINT('Ctrl Pts',(1.79142458548153,4.87182528202395,2.86406713272549));
#10786=CARTESIAN_POINT('Ctrl Pts',(1.81778158504737,4.86793402744908,2.92734810008913));
#10787=CARTESIAN_POINT('Ctrl Pts',(1.84073598285911,4.8640427728742,2.99179776191044));
#10788=CARTESIAN_POINT('Ctrl Pts',(1.86371507458946,4.86014733215929,3.05631675749151));
#10789=CARTESIAN_POINT('Ctrl Pts',(1.88328409647504,4.85625189144437,3.12200648773898));
#10790=CARTESIAN_POINT('Ctrl Pts',(1.89934352177934,4.85235645072946,3.18847161390109));
#10791=CARTESIAN_POINT('Ctrl Pts',(1.91541329890123,4.8484584990348,3.25497958311947));
#10792=CARTESIAN_POINT('Ctrl Pts',(1.92796888898634,4.84456054734014,3.32226345550801));
#10793=CARTESIAN_POINT('Ctrl Pts',(1.9369622120323,4.84066259564547,3.38991944200186));
#10794=CARTESIAN_POINT('Ctrl Pts',(1.9459703877051,4.83675820641692,3.4576871635146));
#10795=CARTESIAN_POINT('Ctrl Pts',(1.9514045239227,4.83285381718836,3.52582773192098));
#10796=CARTESIAN_POINT('Ctrl Pts',(1.95326856711042,4.8289494279598,3.59393509362967));
#10797=CARTESIAN_POINT('Ctrl Pts',(1.95375867881703,4.82792284934794,3.61184251954123));
#10798=CARTESIAN_POINT('Ctrl Pts',(1.95400226243369,4.82689627073609,3.62974767089841));
#10799=CARTESIAN_POINT('Ctrl Pts',(1.95399998416515,4.82586969212423,3.6476432303685));
#10800=CARTESIAN_POINT('Ctrl Pts',(1.95710318190607,4.72413079030316,3.64776998461591));
#10801=CARTESIAN_POINT('Ctrl Pts',(1.95541360145849,4.75994664419965,3.02236479651099));
#10802=CARTESIAN_POINT('Ctrl Pts',(1.29210840943673,4.83277167828651,1.74764265246944));
#10803=CARTESIAN_POINT('Ctrl Pts',(-0.878268351030347,4.94260589256373,
1.51220654580568));
#10804=CARTESIAN_POINT('Ctrl Pts',(-2.26979830067417,5.05363343313481,3.22502187308484));
#10805=CARTESIAN_POINT('Ctrl Pts',(-1.5875322833648,5.16466097370589,5.3237364314922));
#10806=CARTESIAN_POINT('Ctrl Pts',(0.545177970067398,5.27568851427696,5.89086615319871));
#10807=CARTESIAN_POINT('Ctrl Pts',(1.81852615233383,5.36217802636004,4.735922224886));
#10808=CARTESIAN_POINT('Ctrl Pts',(1.95368429139157,5.41165835825274,3.86808546352169));
#10809=CARTESIAN_POINT('Ctrl Pts',(1.95213885961564,5.42412950995508,3.64888667332462));
#10810=CARTESIAN_POINT('Origin',(0.,0.,3.64739446828387));
#10811=CARTESIAN_POINT('',(1.95353597714873,6.22586985342116,3.64632535240867));
#10812=CARTESIAN_POINT('',(1.95399955699052,6.12413030792733,3.64607868681972));
#10813=CARTESIAN_POINT('',(1.954,4.33875158023511E-16,3.64739446828387));
#10814=CARTESIAN_POINT('Ctrl Pts',(1.95399970893239,6.22586969212423,3.64632793551614));
#10815=CARTESIAN_POINT('Ctrl Pts',(1.95403757522787,6.22192922025797,3.71570295389059));
#10816=CARTESIAN_POINT('Ctrl Pts',(1.95037645685081,6.21798874839172,3.78509205096178));
#10817=CARTESIAN_POINT('Ctrl Pts',(1.94303829200873,6.21404827652546,3.8540782745866));
#10818=CARTESIAN_POINT('Ctrl Pts',(1.93569906479725,6.21010723418459,3.92307448556584));
#10819=CARTESIAN_POINT('Ctrl Pts',(1.92468178589055,6.20616619184372,3.99166723064893));
#10820=CARTESIAN_POINT('Ctrl Pts',(1.91006015343091,6.20222514950286,4.05944569116215));
#10821=CARTESIAN_POINT('Ctrl Pts',(1.89541999607838,6.19827911405418,4.12731002366842));
#10822=CARTESIAN_POINT('Ctrl Pts',(1.8771664669629,6.1943330786055,4.19435754146491));
#10823=CARTESIAN_POINT('Ctrl Pts',(1.85542408294095,6.19038704315682,4.26018927280064));
#10824=CARTESIAN_POINT('Ctrl Pts',(1.83366809728879,6.18643853914191,4.32606218724052));
#10825=CARTESIAN_POINT('Ctrl Pts',(1.80841908414587,6.182490035127,4.39071735315611));
#10826=CARTESIAN_POINT('Ctrl Pts',(1.77984999050241,6.17854153111209,4.45377527863874));
#10827=CARTESIAN_POINT('Ctrl Pts',(1.75122193840221,6.17458487851165,4.51696333768521));
#10828=CARTESIAN_POINT('Ctrl Pts',(1.71926033568422,6.17062822591121,4.57854714271363));
#10829=CARTESIAN_POINT('Ctrl Pts',(1.68418427929645,6.16667157331077,4.63817159426665));
#10830=CARTESIAN_POINT('Ctrl Pts',(1.65232394988155,6.16307766144574,4.69232975408544));
#10831=CARTESIAN_POINT('Ctrl Pts',(1.61789476739731,6.15948374958072,4.74487148430728));
#10832=CARTESIAN_POINT('Ctrl Pts',(1.58109015814158,6.15588983771569,4.79555382648631));
#10833=CARTESIAN_POINT('Ctrl Pts',(1.54101347268038,6.15197641278597,4.85074203054611));
#10834=CARTESIAN_POINT('Ctrl Pts',(1.49796252247796,6.14806298785625,4.90394126259874));
#10835=CARTESIAN_POINT('Ctrl Pts',(1.45216195437618,6.14414956292653,4.95481240385855));
#10836=CARTESIAN_POINT('Ctrl Pts',(1.40643121462749,6.14024210447341,5.00560598608009));
#10837=CARTESIAN_POINT('Ctrl Pts',(1.35795950337589,6.13633464602028,5.05407815776852));
#10838=CARTESIAN_POINT('Ctrl Pts',(1.30701347514832,6.13242718756716,5.09992046659878));
#10839=CARTESIAN_POINT('Ctrl Pts',(1.2561284283943,6.12852440627108,5.1457079030152));
#10840=CARTESIAN_POINT('Ctrl Pts',(1.20277531117035,6.12462162497499,5.18887139966879));
#10841=CARTESIAN_POINT('Ctrl Pts',(1.14725832432907,6.12071884367891,5.22913854911921));
#10842=CARTESIAN_POINT('Ctrl Pts',(1.09177680681312,6.11681855583622,5.26937997223424));
#10843=CARTESIAN_POINT('Ctrl Pts',(1.03413456015336,6.11291826799353,5.30672842959029));
#10844=CARTESIAN_POINT('Ctrl Pts',(0.974668408497103,6.10901798015085,5.34095211226229));
#10845=CARTESIAN_POINT('Ctrl Pts',(0.915219717759489,6.10511883754132,5.3751657459077));
#10846=CARTESIAN_POINT('Ctrl Pts',(0.853948612355341,6.10121969493179,5.40625618021199));
#10847=CARTESIAN_POINT('Ctrl Pts',(0.791218844617371,6.09732055232226,5.4340362174665));
#10848=CARTESIAN_POINT('Ctrl Pts',(0.728485838336562,6.09342120841212,5.46181768891794));
#10849=CARTESIAN_POINT('Ctrl Pts',(0.664294472261032,6.08952186450199,5.48628822667285));
#10850=CARTESIAN_POINT('Ctrl Pts',(0.599029234793864,6.08562252059185,5.5073084383003));
#10851=CARTESIAN_POINT('Ctrl Pts',(0.533694725717585,6.08171903797269,5.52835096048602));
#10852=CARTESIAN_POINT('Ctrl Pts',(0.467284540993296,6.07781555535353,5.54593569663892));
#10853=CARTESIAN_POINT('Ctrl Pts',(0.400198132892293,6.07391207273437,5.55997321291885));
#10854=CARTESIAN_POINT('Ctrl Pts',(0.333071752208107,6.07000626427473,5.57401909327436));
#10855=CARTESIAN_POINT('Ctrl Pts',(0.265268833825228,6.06610045581509,5.58451347230028));
#10856=CARTESIAN_POINT('Ctrl Pts',(0.197196009186804,6.06219464735545,5.59141857666339));
#10857=CARTESIAN_POINT('Ctrl Pts',(0.129005325724356,6.05828207652045,5.5983356362742));
#10858=CARTESIAN_POINT('Ctrl Pts',(0.0605442957417832,6.05436950568546,
5.60165099501346));
#10859=CARTESIAN_POINT('Ctrl Pts',(-0.00777927282300132,6.05045693485046,
5.60137898278606));
#10860=CARTESIAN_POINT('Ctrl Pts',(-0.0403448696313994,6.04859205561518,
5.60124933147084));
#10861=CARTESIAN_POINT('Ctrl Pts',(-0.0728792977296982,6.04672717637989,
5.60030545174067));
#10862=CARTESIAN_POINT('Ctrl Pts',(-0.105338970147305,6.04486229714461,
5.59855302190485));
#10863=CARTESIAN_POINT('Ctrl Pts',(-0.173561813075235,6.04094274547719,
5.59486981327928));
#10864=CARTESIAN_POINT('Ctrl Pts',(-0.241725674141963,6.03702319380978,
5.58759689429551));
#10865=CARTESIAN_POINT('Ctrl Pts',(-0.309422647205287,6.03310364214236,
5.57673985607644));
#10866=CARTESIAN_POINT('Ctrl Pts',(-0.377017944907859,6.02918997732352,
5.56589912424787));
#10867=CARTESIAN_POINT('Ctrl Pts',(-0.44414726494164,6.02527631250469,5.55148503414066));
#10868=CARTESIAN_POINT('Ctrl Pts',(-0.510405798910999,6.02136264768585,
5.53355509782687));
#10869=CARTESIAN_POINT('Ctrl Pts',(-0.576586629003742,6.01745357256905,
5.51564618862423));
#10870=CARTESIAN_POINT('Ctrl Pts',(-0.641898229039365,6.01354449745225,
5.49422974987089));
#10871=CARTESIAN_POINT('Ctrl Pts',(-0.705945795963749,6.00963542233545,
5.46941437299433));
#10872=CARTESIAN_POINT('Ctrl Pts',(-0.769953340349426,6.00572878995172,
5.4446145029423));
#10873=CARTESIAN_POINT('Ctrl Pts',(-0.832697961298485,6.001822157568,5.41642008531667));
#10874=CARTESIAN_POINT('Ctrl Pts',(-0.893801338936124,5.99791552518427,
5.38498911794069));
#10875=CARTESIAN_POINT('Ctrl Pts',(-0.954887447690772,5.99400999688317,
5.3535670335057));
#10876=CARTESIAN_POINT('Ctrl Pts',(-1.01433279715199,5.99010446858207,5.31891043993488));
#10877=CARTESIAN_POINT('Ctrl Pts',(-1.07178198514885,5.98619894028097,5.28122413391931));
#10878=CARTESIAN_POINT('Ctrl Pts',(-1.12923459948064,5.98229317904972,5.24353558024957));
#10879=CARTESIAN_POINT('Ctrl Pts',(-1.18469040646407,5.97838741781847,5.20281722710281));
#10880=CARTESIAN_POINT('Ctrl Pts',(-1.23782293994499,5.97448165658721,5.15931720749575));
#10881=CARTESIAN_POINT('Ctrl Pts',(-1.29101183163741,5.97057175247583,5.11577104698133));
#10882=CARTESIAN_POINT('Ctrl Pts',(-1.34187215084897,5.96666184836444,5.06943764360133));
#10883=CARTESIAN_POINT('Ctrl Pts',(-1.39011129021989,5.96275194425305,5.02060479478276));
#10884=CARTESIAN_POINT('Ctrl Pts',(-1.4383792714137,5.95883970243906,4.97174274916685));
#10885=CARTESIAN_POINT('Ctrl Pts',(-1.48402262717635,5.95492746062506,4.920378651296));
#10886=CARTESIAN_POINT('Ctrl Pts',(-1.52678824140386,5.95101521881107,4.86683436672533));
#10887=CARTESIAN_POINT('Ctrl Pts',(-1.56962724054416,5.94709626367074,4.81319820126567));
#10888=CARTESIAN_POINT('Ctrl Pts',(-1.60957835661129,5.94317730853041,4.75737478184416));
#10889=CARTESIAN_POINT('Ctrl Pts',(-1.64643158878374,5.93925835339007,4.69971524801554));
#10890=CARTESIAN_POINT('Ctrl Pts',(-1.66343247001633,5.93745048778456,4.67311614588089));
#10891=CARTESIAN_POINT('Ctrl Pts',(-1.67977473443788,5.93564262217904,4.64612664650909));
#10892=CARTESIAN_POINT('Ctrl Pts',(-1.69544115163435,5.93383475657353,4.61878280532771));
#10893=CARTESIAN_POINT('Ctrl Pts',(-1.72940432509507,5.9299154907718,4.55950418345271));
#10894=CARTESIAN_POINT('Ctrl Pts',(-1.76032172067742,5.92599622497007,4.49832553361439));
#10895=CARTESIAN_POINT('Ctrl Pts',(-1.78797652885598,5.92207695916834,4.43559236999391));
#10896=CARTESIAN_POINT('Ctrl Pts',(-1.81558989213884,5.91816356697678,4.37295322146865));
#10897=CARTESIAN_POINT('Ctrl Pts',(-1.83995017544407,5.91425017478521,4.30876462905162));
#10898=CARTESIAN_POINT('Ctrl Pts',(-1.86088584978545,5.91033678259365,4.24339770155386));
#10899=CARTESIAN_POINT('Ctrl Pts',(-1.88179708321254,5.90642795900979,4.17810708530581));
#10900=CARTESIAN_POINT('Ctrl Pts',(-1.8992914986264,5.90251913542594,4.11164133195107));
#10901=CARTESIAN_POINT('Ctrl Pts',(-1.91324589168175,5.89861031184208,4.04439088887596));
#10902=CARTESIAN_POINT('Ctrl Pts',(-1.9271916116718,5.89470391770693,3.97718224392716));
#10903=CARTESIAN_POINT('Ctrl Pts',(-1.93760157433051,5.89079752357178,3.90919035696625));
#10904=CARTESIAN_POINT('Ctrl Pts',(-1.94440301405618,5.88689112943662,3.84081866255448));
#10905=CARTESIAN_POINT('Ctrl Pts',(-1.9512025553041,5.8829858256886,3.77246605265214));
#10906=CARTESIAN_POINT('Ctrl Pts',(-1.95439552460935,5.87908052194059,3.7037343346659));
#10907=CARTESIAN_POINT('Ctrl Pts',(-1.95396089951249,5.87517521819256,3.6350331100915));
#10908=CARTESIAN_POINT('Ctrl Pts',(-1.95352624692107,5.87126966739347,3.5663275394502));
#10909=CARTESIAN_POINT('Ctrl Pts',(-1.94946355000495,5.86736411659438,3.49765295755817));
#10910=CARTESIAN_POINT('Ctrl Pts',(-1.94180388956302,5.86345856579528,3.42941819783696));
#10911=CARTESIAN_POINT('Ctrl Pts',(-1.93413605902316,5.85954884918065,3.36111065621202));
#10912=CARTESIAN_POINT('Ctrl Pts',(-1.92286366321737,5.85563913256602,3.29324436238369));
#10913=CARTESIAN_POINT('Ctrl Pts',(-1.90806947589916,5.85172941595138,3.2262212555294));
#10914=CARTESIAN_POINT('Ctrl Pts',(-1.89326639420659,5.84781734878633,3.15915785388972));
#10915=CARTESIAN_POINT('Ctrl Pts',(-1.87493743823184,5.84390528162128,3.09293912189492));
#10916=CARTESIAN_POINT('Ctrl Pts',(-1.85321543256441,5.83999321445623,3.0279523317569));
#10917=CARTESIAN_POINT('Ctrl Pts',(-1.83145603003673,5.83607441223037,2.96285365959719));
#10918=CARTESIAN_POINT('Ctrl Pts',(-1.80629209935227,5.83215561000451,2.8989916193083));
#10919=CARTESIAN_POINT('Ctrl Pts',(-1.77790445793065,5.82823680777865,2.83673317127362));
#10920=CARTESIAN_POINT('Ctrl Pts',(-1.76479387842829,5.82642694385325,2.80797966123279));
#10921=CARTESIAN_POINT('Ctrl Pts',(-1.75099633135699,5.82461707992785,2.77956783987734));
#10922=CARTESIAN_POINT('Ctrl Pts',(-1.73653280861798,5.82280721600245,2.75153186464793));
#10923=CARTESIAN_POINT('Ctrl Pts',(-1.7052239763555,5.81888944803674,2.69084307799399));
#10924=CARTESIAN_POINT('Ctrl Pts',(-1.67066771919403,5.81497168007103,2.63167709240382));
#10925=CARTESIAN_POINT('Ctrl Pts',(-1.63303593841815,5.81105391210532,2.57440349728982));
#10926=CARTESIAN_POINT('Ctrl Pts',(-1.59546085757294,5.80714204705379,2.51721619649422));
#10927=CARTESIAN_POINT('Ctrl Pts',(-1.55481971769915,5.80323018200225,2.46191603529419));
#10928=CARTESIAN_POINT('Ctrl Pts',(-1.51133052729588,5.79931831695071,2.40884853160507));
#10929=CARTESIAN_POINT('Ctrl Pts',(-1.46789252609841,5.7954110563828,2.3558434913314));
#10930=CARTESIAN_POINT('Ctrl Pts',(-1.42161344246657,5.79150379581489,2.30506626812456));
#10931=CARTESIAN_POINT('Ctrl Pts',(-1.37275379361176,5.78759653524699,2.25683234377287));
#10932=CARTESIAN_POINT('Ctrl Pts',(-1.32392479182163,5.78369172549627,2.2086286740021));
#10933=CARTESIAN_POINT('Ctrl Pts',(-1.27251878501446,5.77978691574555,2.16296548343151));
#10934=CARTESIAN_POINT('Ctrl Pts',(-1.2188346174519,5.77588210599483,2.12012298773404));
#10935=CARTESIAN_POINT('Ctrl Pts',(-1.16516570144289,5.77197840559195,2.07729266349505));
#10936=CARTESIAN_POINT('Ctrl Pts',(-1.10922029387599,5.76807470518906,2.03728175003944));
#10937=CARTESIAN_POINT('Ctrl Pts',(-1.05133054742944,5.76417100478618,2.00033038937203));
#10938=CARTESIAN_POINT('Ctrl Pts',(-0.993437383134554,5.76026707390628,
1.96337684707222));
#10939=CARTESIAN_POINT('Ctrl Pts',(-0.933600068135027,5.75636314302639,
1.92948347871644));
#10940=CARTESIAN_POINT('Ctrl Pts',(-0.872178434039136,5.75245921214649,
1.89884627644098));
#10941=CARTESIAN_POINT('Ctrl Pts',(-0.810691478933431,5.74855112949318,
1.86817649194885));
#10942=CARTESIAN_POINT('Ctrl Pts',(-0.747617283319028,5.74464304683987,
1.8407700043208));
#10943=CARTESIAN_POINT('Ctrl Pts',(-0.683337987343935,5.74073496418656,
1.8167756671533));
#10944=CARTESIAN_POINT('Ctrl Pts',(-0.619020201144726,5.73682454138663,
1.79276696225819));
#10945=CARTESIAN_POINT('Ctrl Pts',(-0.553496347862654,5.7329141185867,1.7721746216137));
#10946=CARTESIAN_POINT('Ctrl Pts',(-0.487163454161461,5.72900369578677,
1.75509751248399));
#10947=CARTESIAN_POINT('Ctrl Pts',(-0.420716293815641,5.72508653679809,
1.73799098591369));
#10948=CARTESIAN_POINT('Ctrl Pts',(-0.353457793522332,5.72116937780941,
1.7244118735935));
#10949=CARTESIAN_POINT('Ctrl Pts',(-0.285794006257928,5.71725221882073,
1.71440771561663));
#10950=CARTESIAN_POINT('Ctrl Pts',(-0.254283668215943,5.71542803769094,
1.70974888092201));
#10951=CARTESIAN_POINT('Ctrl Pts',(-0.222685489647666,5.71360385656116,
1.70586459717763));
#10952=CARTESIAN_POINT('Ctrl Pts',(-0.191040535300942,5.71177967543137,
1.70275580933668));
#10953=CARTESIAN_POINT('Ctrl Pts',(-0.1230611042813,5.70786098451083,1.69607753683001));
#10954=CARTESIAN_POINT('Ctrl Pts',(-0.0545967376771535,5.70394229359028,
1.69295492978579));
#10955=CARTESIAN_POINT('Ctrl Pts',(0.0139486777056309,5.70002360266974,
1.69344425540989));
#10956=CARTESIAN_POINT('Ctrl Pts',(0.0823910661357122,5.69611080172421,
1.69393284555478));
#10957=CARTESIAN_POINT('Ctrl Pts',(0.150913773809587,5.69219800077868,1.69802259030236));
#10958=CARTESIAN_POINT('Ctrl Pts',(0.219108106246929,5.68828519983315,1.70571796644921));
#10959=CARTESIAN_POINT('Ctrl Pts',(0.287222442472813,5.68437698884753,1.71340431543918));
#10960=CARTESIAN_POINT('Ctrl Pts',(0.355008682185071,5.68046877786191,1.72468784075316));
#10961=CARTESIAN_POINT('Ctrl Pts',(0.42206028141137,5.67656056687629,1.73952101366091));
#10962=CARTESIAN_POINT('Ctrl Pts',(0.489069978092514,5.67265479824833,1.75434491687629));
#10963=CARTESIAN_POINT('Ctrl Pts',(0.555345465977129,5.66874902962038,1.77271396128303));
#10964=CARTESIAN_POINT('Ctrl Pts',(0.620489011696533,5.66484326099242,1.79452928528651));
#10965=CARTESIAN_POINT('Ctrl Pts',(0.685614171468399,5.6609385947186,1.81633845218879));
#10966=CARTESIAN_POINT('Ctrl Pts',(0.749607557262514,5.65703392844478,1.84159181166391));
#10967=CARTESIAN_POINT('Ctrl Pts',(0.812087004737327,5.65312926217096,1.87014077318664));
#10968=CARTESIAN_POINT('Ctrl Pts',(0.874570228709034,5.64922435988417,1.89869146031786));
#10969=CARTESIAN_POINT('Ctrl Pts',(0.93553888652736,5.64531945759738,1.93053793828093));
#10970=CARTESIAN_POINT('Ctrl Pts',(0.99463285904909,5.64141455531059,1.96548440062275));
#10971=CARTESIAN_POINT('Ctrl Pts',(1.05378968769378,5.63750549952036,2.00046803425363));
#10972=CARTESIAN_POINT('Ctrl Pts',(1.11106742756554,5.63359644373013,2.03855798189388));
#10973=CARTESIAN_POINT('Ctrl Pts',(1.16613342782562,5.62968738793989,2.07951410661476));
#10974=CARTESIAN_POINT('Ctrl Pts',(1.22123242710567,5.62577598959692,2.12049477482838));
#10975=CARTESIAN_POINT('Ctrl Pts',(1.27411667037651,5.62186459125394,2.16434472458715));
#10976=CARTESIAN_POINT('Ctrl Pts',(1.32448739361204,5.61795319291096,2.21078417173063));
#10977=CARTESIAN_POINT('Ctrl Pts',(1.37494478129112,5.61403506488178,2.25730351943117));
#10978=CARTESIAN_POINT('Ctrl Pts',(1.42287967463537,5.61011693685261,2.30642090478317));
#10979=CARTESIAN_POINT('Ctrl Pts',(1.46803150387258,5.60619880882343,2.35782108780581));
#10980=CARTESIAN_POINT('Ctrl Pts',(1.4889536798763,5.60438325083572,2.38163858742855));
#10981=CARTESIAN_POINT('Ctrl Pts',(1.50927887683722,5.602567692848,2.4059457964163));
#10982=CARTESIAN_POINT('Ctrl Pts',(1.5289843240469,5.60075213486029,2.43070924324872));
#10983=CARTESIAN_POINT('Ctrl Pts',(1.571427375016,5.59684165166293,2.48404658824245));
#10984=CARTESIAN_POINT('Ctrl Pts',(1.61116405275229,5.59293116846557,2.5397180074941));
#10985=CARTESIAN_POINT('Ctrl Pts',(1.6479272127628,5.58902068526822,2.59741737261186));
#10986=CARTESIAN_POINT('Ctrl Pts',(1.68463680664051,5.58511589987981,2.65503266628818));
#10987=CARTESIAN_POINT('Ctrl Pts',(1.71838121312421,5.58121111449141,2.71466963328221));
#10988=CARTESIAN_POINT('Ctrl Pts',(1.74893386808947,5.577306329103,2.7759896685211));
#10989=CARTESIAN_POINT('Ctrl Pts',(1.77945257014948,5.57340588306934,2.83724155932709));
#10990=CARTESIAN_POINT('Ctrl Pts',(1.80678633979274,5.56950543703568,2.90017236789852));
#10991=CARTESIAN_POINT('Ctrl Pts',(1.83075322221469,5.56560499100202,2.9644166945968));
#10992=CARTESIAN_POINT('Ctrl Pts',(1.85470355842854,5.56170723775045,3.028616668426));
#10993=CARTESIAN_POINT('Ctrl Pts',(1.87529144678653,5.55780948449888,3.09412790017339));
#10994=CARTESIAN_POINT('Ctrl Pts',(1.89238272508226,5.55391173124731,3.160564290696));
#10995=CARTESIAN_POINT('Ctrl Pts',(1.90946718207926,5.55001553362773,3.22697416579603));
#10996=CARTESIAN_POINT('Ctrl Pts',(1.92305768028705,5.54611933600815,3.29430798817317));
#10997=CARTESIAN_POINT('Ctrl Pts',(1.93307022193307,5.54222313838858,3.3621655828679));
#10998=CARTESIAN_POINT('Ctrl Pts',(1.94308489345346,5.53832611196731,3.43003761227433));
#10999=CARTESIAN_POINT('Ctrl Pts',(1.94952001575387,5.53442908554603,3.49843314825239));
#11000=CARTESIAN_POINT('Ctrl Pts',(1.95234315435092,5.53053205912476,3.56694443621978));
#11001=CARTESIAN_POINT('Ctrl Pts',(1.95346901347271,5.52897793679125,3.59426653035457));
#11002=CARTESIAN_POINT('Ctrl Pts',(1.95402100669827,5.52742381445774,3.62160699244058));
#11003=CARTESIAN_POINT('Ctrl Pts',(1.95399938885048,5.52586969212423,3.64893990412503));
#11004=CARTESIAN_POINT('Ctrl Pts',(1.95399943981962,5.42413030787577,3.64887405762317));
#11005=CARTESIAN_POINT('Ctrl Pts',(1.9540514551376,5.42803486416929,3.58018073880955));
#11006=CARTESIAN_POINT('Ctrl Pts',(1.95047675797586,5.4319394204628,3.51144725141444));
#11007=CARTESIAN_POINT('Ctrl Pts',(1.94328925495969,5.43584397675632,3.44308374522165));
#11008=CARTESIAN_POINT('Ctrl Pts',(1.93610276751857,5.43974798134642,3.37472989861037));
#11009=CARTESIAN_POINT('Ctrl Pts',(1.92530453973603,5.44365198593652,3.30674641766519));
#11010=CARTESIAN_POINT('Ctrl Pts',(1.91096035466864,5.44755599052662,3.23953846074605));
#11011=CARTESIAN_POINT('Ctrl Pts',(1.89661329756237,5.45146077678908,3.17231704723357));
#11012=CARTESIAN_POINT('Ctrl Pts',(1.87871897897927,5.45536556305154,3.10587194559488));
#11013=CARTESIAN_POINT('Ctrl Pts',(1.85739392663886,5.459270349314,3.04059647777544));
#11014=CARTESIAN_POINT('Ctrl Pts',(1.83604304214031,5.46317986564955,2.97524193834669));
#11015=CARTESIAN_POINT('Ctrl Pts',(1.81125328691822,5.46708938198511,2.91106032641277));
#11016=CARTESIAN_POINT('Ctrl Pts',(1.78319022584856,5.47099889832066,2.84842724840677));
#11017=CARTESIAN_POINT('Ctrl Pts',(1.7551069686539,5.4749112282153,2.78574909529402));
#11018=CARTESIAN_POINT('Ctrl Pts',(1.72374594392167,5.47882355810995,2.72462212920007));
#11019=CARTESIAN_POINT('Ctrl Pts',(1.68931847990919,5.48273588800459,2.66539697672022));
#11020=CARTESIAN_POINT('Ctrl Pts',(1.65483066125898,5.48665507658779,2.60606799688262));
#11021=CARTESIAN_POINT('Ctrl Pts',(1.61726594887417,5.490574265171,2.54864789067694));
#11022=CARTESIAN_POINT('Ctrl Pts',(1.57687814704101,5.4944934537542,2.49345716089473));
#11023=CARTESIAN_POINT('Ctrl Pts',(1.56571375465843,5.49557683430917,2.47820079795339));
#11024=CARTESIAN_POINT('Ctrl Pts',(1.55433386759307,5.49666021486415,2.46311458302517));
#11025=CARTESIAN_POINT('Ctrl Pts',(1.54274435158161,5.49774359541912,2.44820479785512));
#11026=CARTESIAN_POINT('Ctrl Pts',(1.50082572987124,5.5016621214048,2.39427695102281));
#11027=CARTESIAN_POINT('Ctrl Pts',(1.45599318072079,5.50558064739048,2.34244306268919));
#11028=CARTESIAN_POINT('Ctrl Pts',(1.40848368839703,5.50949917337616,2.29303495193694));
#11029=CARTESIAN_POINT('Ctrl Pts',(1.36104562422435,5.51341180805355,2.24370112381383));
#11030=CARTESIAN_POINT('Ctrl Pts',(1.31093894257671,5.51732444273093,2.19678618675944));
#11031=CARTESIAN_POINT('Ctrl Pts',(1.25844152415245,5.52123707740832,2.15258982208797));
#11032=CARTESIAN_POINT('Ctrl Pts',(1.20600570638572,5.52514512098626,2.10844531758802));
#11033=CARTESIAN_POINT('Ctrl Pts',(1.1511850976712,5.5290531645642,2.06701336528422));
#11034=CARTESIAN_POINT('Ctrl Pts',(1.09429384419979,5.53296120814213,2.02855631005234));
#11035=CARTESIAN_POINT('Ctrl Pts',(1.03743815411931,5.53686680875612,1.9901232947775));
#11036=CARTESIAN_POINT('Ctrl Pts',(0.978514793457789,5.5407724093701,1.95466176237224));
#11037=CARTESIAN_POINT('Ctrl Pts',(0.917869103633709,5.54467800998409,1.92239234985194));
#11038=CARTESIAN_POINT('Ctrl Pts',(0.857240536397379,5.54858250789828,1.89013204821568));
#11039=CARTESIAN_POINT('Ctrl Pts',(0.794891039285684,5.55248700581248,1.86106230817246));
#11040=CARTESIAN_POINT('Ctrl Pts',(0.731191334976556,5.55639150372668,1.83535825682031));
#11041=CARTESIAN_POINT('Ctrl Pts',(0.667487781642525,5.56029623756834,1.80965265231286));
#11042=CARTESIAN_POINT('Ctrl Pts',(0.602434316124245,5.56420097141,1.78731332188365));
#11043=CARTESIAN_POINT('Ctrl Pts',(0.536420762696227,5.56810570525167,1.76846691104586));
#11044=CARTESIAN_POINT('Ctrl Pts',(0.47033697254014,5.57201459363001,1.74960044811022));
#11045=CARTESIAN_POINT('Ctrl Pts',(0.403291529646144,5.57592348200835,1.73423445667258));
#11046=CARTESIAN_POINT('Ctrl Pts',(0.335687534544171,5.57983237038669,1.72244514969087));
#11047=CARTESIAN_POINT('Ctrl Pts',(0.268043019113123,5.58374360166567,1.71064877646112));
#11048=CARTESIAN_POINT('Ctrl Pts',(0.199839773474815,5.58765483294465,1.70243341304384));
#11049=CARTESIAN_POINT('Ctrl Pts',(0.131486358980064,5.59156606422363,1.69782340330517));
#11050=CARTESIAN_POINT('Ctrl Pts',(0.0630152951561597,5.5954840274814,1.69320545885605));
#11051=CARTESIAN_POINT('Ctrl Pts',(-0.00560596196028167,5.59940199073916,
1.69220526025078));
#11052=CARTESIAN_POINT('Ctrl Pts',(-0.0739693956144667,5.60331995399692,
1.69479503969837));
#11053=CARTESIAN_POINT('Ctrl Pts',(-0.105674773640132,5.60513701466135,
1.69599611945695));
#11054=CARTESIAN_POINT('Ctrl Pts',(-0.137324779937373,5.60695407532578,
1.69796863240154));
#11055=CARTESIAN_POINT('Ctrl Pts',(-0.168879356249839,5.6087711359902,1.70070605895056));
#11056=CARTESIAN_POINT('Ctrl Pts',(-0.236924946485957,5.6126895205751,1.70660915850138));
#11057=CARTESIAN_POINT('Ctrl Pts',(-0.304795263666282,5.61660790515999,
1.71609598339349));
#11058=CARTESIAN_POINT('Ctrl Pts',(-0.37208300607575,5.62052628974489,1.72914781141473));
#11059=CARTESIAN_POINT('Ctrl Pts',(-0.439269574640891,5.62443878264702,
1.74218001470835));
#11060=CARTESIAN_POINT('Ctrl Pts',(-0.505874827988365,5.62835127554915,
1.7587664897847));
#11061=CARTESIAN_POINT('Ctrl Pts',(-0.571496231559392,5.63226376845129,
1.77883672036345));
#11062=CARTESIAN_POINT('Ctrl Pts',(-0.637040634203744,5.63617167038824,
1.79888340029762));
#11063=CARTESIAN_POINT('Ctrl Pts',(-0.701603011786067,5.64007957232519,
1.82240557394209));
#11064=CARTESIAN_POINT('Ctrl Pts',(-0.764792477692609,5.64398747426214,
1.84928199514299));
#11065=CARTESIAN_POINT('Ctrl Pts',(-0.827942444368853,5.64789293340081,
1.87614161610773));
#11066=CARTESIAN_POINT('Ctrl Pts',(-0.889720750222587,5.65179839253948,
1.90635113331962));
#11067=CARTESIAN_POINT('Ctrl Pts',(-0.949754581589428,5.65570385167816,
1.93974045334118));
#11068=CARTESIAN_POINT('Ctrl Pts',(-1.00977146830455,5.6596082084943,1.97312034916998));
#11069=CARTESIAN_POINT('Ctrl Pts',(-1.06804442841452,5.66351256531044,2.00967802715169));
#11070=CARTESIAN_POINT('Ctrl Pts',(-1.12422507203602,5.66741692212658,2.04919736297877));
#11071=CARTESIAN_POINT('Ctrl Pts',(-1.18040911894683,5.67132151545933,2.08871909279289));
#11072=CARTESIAN_POINT('Ctrl Pts',(-1.23450019697194,5.67522610879209,2.13120255158595));
#11073=CARTESIAN_POINT('Ctrl Pts',(-1.28618024652872,5.67913070212485,2.17638924278692));
#11074=CARTESIAN_POINT('Ctrl Pts',(-1.33791530868143,5.6830394518355,2.22162403450649));
#11075=CARTESIAN_POINT('Ctrl Pts',(-1.38723384954957,5.68694820154615,2.26956747692651));
#11076=CARTESIAN_POINT('Ctrl Pts',(-1.43385294230865,5.6908569512568,2.31992253267362));
#11077=CARTESIAN_POINT('Ctrl Pts',(-1.48049998864117,5.69476804471795,2.37030778213891));
#11078=CARTESIAN_POINT('Ctrl Pts',(-1.52444405084831,5.6986791381791,2.42310714477325));
#11079=CARTESIAN_POINT('Ctrl Pts',(-1.56544278673989,5.70259023164025,2.47799082477833));
#11080=CARTESIAN_POINT('Ctrl Pts',(-1.60651212056007,5.7065080598236,2.53296901194412));
#11081=CARTESIAN_POINT('Ctrl Pts',(-1.64462573292539,5.71042588800695,2.59003827088932));
#11082=CARTESIAN_POINT('Ctrl Pts',(-1.67958533188183,5.71434371619031,2.6488409579864));
#11083=CARTESIAN_POINT('Ctrl Pts',(-1.69581058202618,5.71616203631396,2.67613212652923));
#11084=CARTESIAN_POINT('Ctrl Pts',(-1.71135711117398,5.71798035643762,2.70379635134295));
#11085=CARTESIAN_POINT('Ctrl Pts',(-1.72620860178437,5.71979867656128,2.73179637789395));
#11086=CARTESIAN_POINT('Ctrl Pts',(-1.75821443653912,5.7237172632497,2.79213808004562));
#11087=CARTESIAN_POINT('Ctrl Pts',(-1.78711577385684,5.72763584993812,2.85427932151719));
#11088=CARTESIAN_POINT('Ctrl Pts',(-1.8127070947079,5.73155443662653,2.91786791715934));
#11089=CARTESIAN_POINT('Ctrl Pts',(-1.83825993473054,5.73546713106488,2.98136089671926));
#11090=CARTESIAN_POINT('Ctrl Pts',(-1.86051245417097,5.73937982550323,3.04629645861358));
#11091=CARTESIAN_POINT('Ctrl Pts',(-1.87930521175737,5.74329251994158,3.11229828902111));
#11092=CARTESIAN_POINT('Ctrl Pts',(-1.89807591022528,5.7472006216218,3.17822264584923));
#11093=CARTESIAN_POINT('Ctrl Pts',(-1.91339477829516,5.75110872330202,3.24521031476371));
#11094=CARTESIAN_POINT('Ctrl Pts',(-1.92515129595695,5.75501682498224,3.31286720829557));
#11095=CARTESIAN_POINT('Ctrl Pts',(-1.93690046140127,5.75892248263828,3.38048179098259));
#11096=CARTESIAN_POINT('Ctrl Pts',(-1.94509161174385,5.76282814029432,3.44876428467494));
#11097=CARTESIAN_POINT('Ctrl Pts',(-1.94966505701588,5.76673379795036,3.51730924448326));
#11098=CARTESIAN_POINT('Ctrl Pts',(-1.95423720971819,5.7706383517701,3.58583483177583));
#11099=CARTESIAN_POINT('Ctrl Pts',(-1.95519365441088,5.77454290558984,3.65462224750134));
#11100=CARTESIAN_POINT('Ctrl Pts',(-1.95252661590114,5.77844745940959,3.72326155072172));
#11101=CARTESIAN_POINT('Ctrl Pts',(-1.94985941706836,5.78235224794284,3.79190498004009));
#11102=CARTESIAN_POINT('Ctrl Pts',(-1.94356832425462,5.78625703647609,3.8603997879099));
#11103=CARTESIAN_POINT('Ctrl Pts',(-1.93369761352118,5.79016182500934,3.92833848310264));
#11104=CARTESIAN_POINT('Ctrl Pts',(-1.9238164062701,5.79407076589625,3.99634942433036));
#11105=CARTESIAN_POINT('Ctrl Pts',(-1.91034805528997,5.79797970678315,4.06380258514305));
#11106=CARTESIAN_POINT('Ctrl Pts',(-1.89338827958256,5.80188864767005,4.13029903726142));
#11107=CARTESIAN_POINT('Ctrl Pts',(-1.87641834377479,5.8057999302879,4.19683532543889));
#11108=CARTESIAN_POINT('Ctrl Pts',(-1.85595296703681,5.80971121290576,4.26241329479919));
#11109=CARTESIAN_POINT('Ctrl Pts',(-1.83213741818948,5.81362249552361,4.32665029701853));
#11110=CARTESIAN_POINT('Ctrl Pts',(-1.80828089286891,5.81754050780235,4.3909978239131));
#11111=CARTESIAN_POINT('Ctrl Pts',(-1.78106288604198,5.82145852008109,4.4539993277038));
#11112=CARTESIAN_POINT('Ctrl Pts',(-1.75067597596649,5.82537653235982,4.51529401729503));
#11113=CARTESIAN_POINT('Ctrl Pts',(-1.73658727746823,5.82719309395067,4.54371291211027));
#11114=CARTESIAN_POINT('Ctrl Pts',(-1.7218180070701,5.82900965554151,4.57176527645755));
#11115=CARTESIAN_POINT('Ctrl Pts',(-1.70639051229435,5.83082621713236,4.59941727239722));
#11116=CARTESIAN_POINT('Ctrl Pts',(-1.67311031083597,5.8347449049416,4.6590681754748));
#11117=CARTESIAN_POINT('Ctrl Pts',(-1.63663272637617,5.83866359275084,4.71708976633959));
#11118=CARTESIAN_POINT('Ctrl Pts',(-1.59714186055193,5.84258228056009,4.77311818095618));
#11119=CARTESIAN_POINT('Ctrl Pts',(-1.55771034837625,5.84649507869296,4.82906238645856));
#11120=CARTESIAN_POINT('Ctrl Pts',(-1.51527482417665,5.85040787682584,4.88301896247169));
#11121=CARTESIAN_POINT('Ctrl Pts',(-1.47006467497902,5.85432067495872,4.93464963000545));
#11122=CARTESIAN_POINT('Ctrl Pts',(-1.42490755490916,5.85822888358513,4.98621973748103));
#11123=CARTESIAN_POINT('Ctrl Pts',(-1.37698259577513,5.86213709221154,5.03546898652687));
#11124=CARTESIAN_POINT('Ctrl Pts',(-1.32656067870836,5.86604530083795,5.08209052170593));
#11125=CARTESIAN_POINT('Ctrl Pts',(-1.27617026817339,5.86995106738943,5.12868292505172));
#11126=CARTESIAN_POINT('Ctrl Pts',(-1.22328635500603,5.87385683394092,5.1726505386083));
#11127=CARTESIAN_POINT('Ctrl Pts',(-1.16821696380806,5.8777626004924,5.21372301794103));
#11128=CARTESIAN_POINT('Ctrl Pts',(-1.11316311124442,5.88166726497472,5.25478390807286));
#11129=CARTESIAN_POINT('Ctrl Pts',(-1.05592539883184,5.88557192945703,5.29295099187465));
#11130=CARTESIAN_POINT('Ctrl Pts',(-0.996843822961217,5.88947659393935,
5.32799507301543));
#11131=CARTESIAN_POINT('Ctrl Pts',(-0.937758671622232,5.89338149472214,
5.36304127493584));
#11132=CARTESIAN_POINT('Ctrl Pts',(-0.876829859508176,5.89728639550492,
5.39496385033971));
#11133=CARTESIAN_POINT('Ctrl Pts',(-0.814423597313302,5.90119129628771,
5.42357863782803));
#11134=CARTESIAN_POINT('Ctrl Pts',(-0.751950948727575,5.90510035101692,
5.45222386508953));
#11135=CARTESIAN_POINT('Ctrl Pts',(-0.68799816132685,5.90900940574613,5.47755407684457));
#11136=CARTESIAN_POINT('Ctrl Pts',(-0.622952197243925,5.91291846047534,
5.49943295599112));
#11137=CARTESIAN_POINT('Ctrl Pts',(-0.557867249321767,5.9168298580088,5.52132494775303));
#11138=CARTESIAN_POINT('Ctrl Pts',(-0.49168829452493,5.92074125554226,5.53976135825024));
#11139=CARTESIAN_POINT('Ctrl Pts',(-0.424815539001397,5.92465265307572,
5.55465631654251));
#11140=CARTESIAN_POINT('Ctrl Pts',(-0.357827719992853,5.92857078068973,
5.5695769035949));
#11141=CARTESIAN_POINT('Ctrl Pts',(-0.290144202343355,5.93248890830375,
5.58094379549636));
#11142=CARTESIAN_POINT('Ctrl Pts',(-0.222172536782913,5.93640703591776,
5.58872271561853));
#11143=CARTESIAN_POINT('Ctrl Pts',(-0.190675965964007,5.93822260984632,
5.59232729565202));
#11144=CARTESIAN_POINT('Ctrl Pts',(-0.159117552570487,5.94003818377488,
5.5951622042778));
#11145=CARTESIAN_POINT('Ctrl Pts',(-0.127537778503509,5.94185375770344,
5.59722782399774));
#11146=CARTESIAN_POINT('Ctrl Pts',(-0.0593934976570972,5.94577148616542,
5.60168511270469));
#11147=CARTESIAN_POINT('Ctrl Pts',(0.00911979872288664,5.9496892146274,
5.60257459642064));
#11148=CARTESIAN_POINT('Ctrl Pts',(0.0775967852891967,5.95360694308939,
5.59985310777224));
#11149=CARTESIAN_POINT('Ctrl Pts',(0.145970770506179,5.95751877860341,5.59713571271816));
#11150=CARTESIAN_POINT('Ctrl Pts',(0.214308066663938,5.96143061411744,5.59081814430954));
#11151=CARTESIAN_POINT('Ctrl Pts',(0.282200215529573,5.96534244963147,5.58090915360567));
#11152=CARTESIAN_POINT('Ctrl Pts',(0.350012708166729,5.96924969548279,5.57101178888272));
#11153=CARTESIAN_POINT('Ctrl Pts',(0.417380606241897,5.97315694133412,5.55753144105258));
#11154=CARTESIAN_POINT('Ctrl Pts',(0.483899283144623,5.97706418718544,5.54052876985154));
#11155=CARTESIAN_POINT('Ctrl Pts',(0.550376392945058,5.98096899142344,5.52353672351266));
#11156=CARTESIAN_POINT('Ctrl Pts',(0.616004858668005,5.98487379566144,5.5030268415894));
#11157=CARTESIAN_POINT('Ctrl Pts',(0.68039052408249,5.98877859989944,5.47911080405717));
#11158=CARTESIAN_POINT('Ctrl Pts',(0.744758049056729,5.99268230397225,5.45520150478642));
#11159=CARTESIAN_POINT('Ctrl Pts',(0.807883007867177,5.99658600804505,5.42788812625661));
#11160=CARTESIAN_POINT('Ctrl Pts',(0.869388420972534,6.00048971211786,5.39733154528946));
#11161=CARTESIAN_POINT('Ctrl Pts',(0.930897609891899,6.00439365583885,5.36677308845545));
#11162=CARTESIAN_POINT('Ctrl Pts',(0.990786616269292,6.00829759955984,5.33297125510818));
#11163=CARTESIAN_POINT('Ctrl Pts',(1.0487020315943,6.01220154328083,5.29613339513978));
#11164=CARTESIAN_POINT('Ctrl Pts',(1.10667924245568,6.01610965249549,5.2592562293095));
#11165=CARTESIAN_POINT('Ctrl Pts',(1.16267824386813,6.02001776171016,5.21933683660997));
#11166=CARTESIAN_POINT('Ctrl Pts',(1.21637452603494,6.02392587092482,5.17662597868813));
#11167=CARTESIAN_POINT('Ctrl Pts',(1.27010306932354,6.02783632816028,5.13388945976828));
#11168=CARTESIAN_POINT('Ctrl Pts',(1.3215257716477,6.03174678539575,5.08835846407014));
#11169=CARTESIAN_POINT('Ctrl Pts',(1.37035328888146,6.03565724263121,5.0403222710259));
#11170=CARTESIAN_POINT('Ctrl Pts',(1.41926506327743,6.03957444778359,4.99220318633494));
#11171=CARTESIAN_POINT('Ctrl Pts',(1.46557238303436,6.04349165293597,4.94157063931928));
#11172=CARTESIAN_POINT('Ctrl Pts',(1.50902523794478,6.04740885808835,4.88874809688681));
#11173=CARTESIAN_POINT('Ctrl Pts',(1.52926017077446,6.04923300481707,4.86414992951168));
#11174=CARTESIAN_POINT('Ctrl Pts',(1.54887670810714,6.05105715154579,4.83907727941792));
#11175=CARTESIAN_POINT('Ctrl Pts',(1.56785287850624,6.05288129827452,4.81356484664189));
#11176=CARTESIAN_POINT('Ctrl Pts',(1.6088093661754,6.05681837522051,4.75850106841765));
#11177=CARTESIAN_POINT('Ctrl Pts',(1.64694295803684,6.06075545216651,4.70116771866654));
#11178=CARTESIAN_POINT('Ctrl Pts',(1.68199473772208,6.06469252911251,4.64188413754908));
#11179=CARTESIAN_POINT('Ctrl Pts',(1.71699327098076,6.06862362532714,4.58269061288171));
#11180=CARTESIAN_POINT('Ctrl Pts',(1.74891903684479,6.07255472154176,4.52155314947093));
#11181=CARTESIAN_POINT('Ctrl Pts',(1.77755484817185,6.07648581775638,4.45882207549275));
#11182=CARTESIAN_POINT('Ctrl Pts',(1.80647677722473,6.080456191933,4.39546421737987));
#11183=CARTESIAN_POINT('Ctrl Pts',(1.83204232976779,6.08442656610961,4.33048112322196));
#11184=CARTESIAN_POINT('Ctrl Pts',(1.85407425987923,6.08839694028623,4.2642612601063));
#11185=CARTESIAN_POINT('Ctrl Pts',(1.87584314099761,6.09231991040319,4.1988320253298));
#11186=CARTESIAN_POINT('Ctrl Pts',(1.89416217128954,6.09624288052016,4.13219586906019));
#11187=CARTESIAN_POINT('Ctrl Pts',(1.9089086849859,6.10016585063712,4.06474759500681));
#11188=CARTESIAN_POINT('Ctrl Pts',(1.92392248772374,6.10415992684356,3.99607678219664));
#11189=CARTESIAN_POINT('Ctrl Pts',(1.9352327965442,6.10815400305,3.92656460262292));
#11190=CARTESIAN_POINT('Ctrl Pts',(1.94276391462493,6.11214807925644,3.85664162365573));
#11191=CARTESIAN_POINT('Ctrl Pts',(1.95029503270565,6.11614215546288,3.78671864468854));
#11192=CARTESIAN_POINT('Ctrl Pts',(1.95404689998987,6.12013623166932,3.71638539512167));
#11193=CARTESIAN_POINT('Ctrl Pts',(1.95399955699113,6.12413030787576,3.64607868772759));
#11194=CARTESIAN_POINT('Origin',(0.,0.,3.64739446828387));
#11195=CARTESIAN_POINT('',(-0.834037993952278,6.59995882699137,5.41445321791391));
#11196=CARTESIAN_POINT('Ctrl Pts',(1.95399955699052,6.12413030792734,3.64607868681973));
#11197=CARTESIAN_POINT('Ctrl Pts',(1.95394681966027,6.12857947203199,3.56776118292628));
#11198=CARTESIAN_POINT('Ctrl Pts',(1.9491815174852,6.13302863613665,3.48962762197157));
#11199=CARTESIAN_POINT('Ctrl Pts',(1.93979384649706,6.13747780024131,3.41220128578885));
#11200=CARTESIAN_POINT('Ctrl Pts',(1.93032535002667,6.14196527052806,3.334108328357));
#11201=CARTESIAN_POINT('Ctrl Pts',(1.9161546596225,6.14645274081481,3.25673503473416));
#11202=CARTESIAN_POINT('Ctrl Pts',(1.89742413111215,6.15094021110156,3.18059936690288));
#11203=CARTESIAN_POINT('Ctrl Pts',(1.87938061318503,6.15526308701624,3.10725625292463));
#11204=CARTESIAN_POINT('Ctrl Pts',(1.85710603049997,6.15958596293091,3.03506166685624));
#11205=CARTESIAN_POINT('Ctrl Pts',(1.83076925289313,6.16390883884559,2.96445966710506));
#11206=CARTESIAN_POINT('Ctrl Pts',(1.80688998876339,6.16782834248827,2.90044561704498));
#11207=CARTESIAN_POINT('Ctrl Pts',(1.77960225082737,6.17174784613095,2.83755952478635));
#11208=CARTESIAN_POINT('Ctrl Pts',(1.74903318078107,6.17566734977363,2.77618902034013));
#11209=CARTESIAN_POINT('Ctrl Pts',(1.71850995347514,6.1795809755539,2.7149105498386));
#11210=CARTESIAN_POINT('Ctrl Pts',(1.68471537782719,6.18349460133417,2.65514359264585));
#11211=CARTESIAN_POINT('Ctrl Pts',(1.64782522231823,6.18740822711444,2.59725731691178));
#11212=CARTESIAN_POINT('Ctrl Pts',(1.61097820320366,6.19131727661405,2.53943872875413));
#11213=CARTESIAN_POINT('Ctrl Pts',(1.57104305610025,6.19522632611366,2.48349686699577));
#11214=CARTESIAN_POINT('Ctrl Pts',(1.52824131094056,6.19913537561327,2.42977609804849));
#11215=CARTESIAN_POINT('Ctrl Pts',(1.485466220882,6.20304199072359,2.37608878410457));
#11216=CARTESIAN_POINT('Ctrl Pts',(1.43982837971589,6.20694860583392,2.32462020257675));
#11217=CARTESIAN_POINT('Ctrl Pts',(1.39159154689848,6.21085522094425,2.2756842340869));
#11218=CARTESIAN_POINT('Ctrl Pts',(1.34336824369791,6.21476074031502,2.22676199130964));
#11219=CARTESIAN_POINT('Ctrl Pts',(1.29254774089051,6.2186662596858,2.18037130118323));
#11220=CARTESIAN_POINT('Ctrl Pts',(1.239431617202,6.22257177905657,2.1367901963847));
#11221=CARTESIAN_POINT('Ctrl Pts',(1.18631221202198,6.22647753970867,2.09320639916406));
#11222=CARTESIAN_POINT('Ctrl Pts',(1.13089728596076,6.23038330036077,2.05243284162792));
#11223=CARTESIAN_POINT('Ctrl Pts',(1.07352113506544,6.23428906101287,2.01470699893531));
#11224=CARTESIAN_POINT('Ctrl Pts',(1.01608394002085,6.23819897711689,1.97694101862565));
#11225=CARTESIAN_POINT('Ctrl Pts',(0.956681767401087,6.2421088932209,1.94222949473817));
#11226=CARTESIAN_POINT('Ctrl Pts',(0.895676657146016,6.24601880932492,1.91076574404724));
#11227=CARTESIAN_POINT('Ctrl Pts',(0.834634960160548,6.24993107033162,1.87928312353116));
#11228=CARTESIAN_POINT('Ctrl Pts',(0.771988860386681,6.25384333133831,1.8510523547138));
#11229=CARTESIAN_POINT('Ctrl Pts',(0.708121117161774,6.257755592345,1.82621889096312));
#11230=CARTESIAN_POINT('Ctrl Pts',(0.644143601749468,6.2616745775199,1.80134274488958));
#11231=CARTESIAN_POINT('Ctrl Pts',(0.578940718830332,6.2655935626948,1.77987571125726));
#11232=CARTESIAN_POINT('Ctrl Pts',(0.512910290448957,6.2695125478697,1.76191335356764));
#11233=CARTESIAN_POINT('Ctrl Pts',(0.482448499574328,6.2713204917187,1.75362678634447));
#11234=CARTESIAN_POINT('Ctrl Pts',(0.451810724361782,6.27312843556769,1.7460853844003));
#11235=CARTESIAN_POINT('Ctrl Pts',(0.421036523795813,6.27493637941668,1.73929482580449));
#11236=CARTESIAN_POINT('Ctrl Pts',(0.354427834596093,6.27884955238994,1.72459711802713));
#11237=CARTESIAN_POINT('Ctrl Pts',(0.286914720102416,6.28276272536319,1.71336187894293));
#11238=CARTESIAN_POINT('Ctrl Pts',(0.218890401956769,6.28667589833644,1.70569341201099));
#11239=CARTESIAN_POINT('Ctrl Pts',(0.150968725339446,6.29058316674401,1.69803651598763));
#11240=CARTESIAN_POINT('Ctrl Pts',(0.0825378619267655,6.29449043515158,
1.69393576663677));
#11241=CARTESIAN_POINT('Ctrl Pts',(0.0140020575316699,6.29839770355914,
1.693444637202));
#11242=CARTESIAN_POINT('Ctrl Pts',(-0.05445332293134,6.30230038694882,1.6929540840873));
#11243=CARTESIAN_POINT('Ctrl Pts',(-0.123012908974516,6.30620307033851,
1.69606474292708));
#11244=CARTESIAN_POINT('Ctrl Pts',(-0.191268328643992,6.31010575372819,
1.70277820113558));
#11245=CARTESIAN_POINT('Ctrl Pts',(-0.259481139672085,6.31400600085657,
1.70948746844856));
#11246=CARTESIAN_POINT('Ctrl Pts',(-0.327389671181108,6.31790624798496,
1.71979502595738));
#11247=CARTESIAN_POINT('Ctrl Pts',(-0.39458814071355,6.32180649511335,1.73365044172018));
#11248=CARTESIAN_POINT('Ctrl Pts',(-0.461767861968078,6.32570565407831,
1.74750199184158));
#11249=CARTESIAN_POINT('Ctrl Pts',(-0.528237431631303,6.32960481304326,
1.7648993357988));
#11250=CARTESIAN_POINT('Ctrl Pts',(-0.593600579199147,6.33350397200822,
1.78574080759012));
#11251=CARTESIAN_POINT('Ctrl Pts',(-0.658968056903733,6.33740338928221,
1.80658366007417));
#11252=CARTESIAN_POINT('Ctrl Pts',(-0.723228497863437,6.3413028065562,1.83087094102833));
#11253=CARTESIAN_POINT('Ctrl Pts',(-0.786001893430877,6.34520222383019,
1.85845147771009));
#11254=CARTESIAN_POINT('Ctrl Pts',(-0.848843289649065,6.34910586523305,
1.88606189161014));
#11255=CARTESIAN_POINT('Ctrl Pts',(-0.910193973351151,6.35300950663591,
1.9169724817724));
#11256=CARTESIAN_POINT('Ctrl Pts',(-0.969695934475925,6.35691314803876,
1.95098479056423));
#11257=CARTESIAN_POINT('Ctrl Pts',(-1.0292340940101,6.36081916424754,1.9850177909678));
#11258=CARTESIAN_POINT('Ctrl Pts',(-1.08692087827315,6.36472518045632,2.02215599775597));
#11259=CARTESIAN_POINT('Ctrl Pts',(-1.14242723508615,6.3686311966651,2.06215757351596));
#11260=CARTESIAN_POINT('Ctrl Pts',(-1.19803072837799,6.37254404842718,2.10222915228894));
#11261=CARTESIAN_POINT('Ctrl Pts',(-1.2514457948728,6.37645690018927,2.14517379158583));
#11262=CARTESIAN_POINT('Ctrl Pts',(-1.30237711460561,6.38036975195135,2.19070992750246));
#11263=CARTESIAN_POINT('Ctrl Pts',(-1.32664912712783,6.38223447463015,2.21241079186215));
#11264=CARTESIAN_POINT('Ctrl Pts',(-1.35035760118794,6.38409919730895,2.23469968813218));
#11265=CARTESIAN_POINT('Ctrl Pts',(-1.37347374173203,6.38596391998775,2.25754344001767));
#11266=CARTESIAN_POINT('Ctrl Pts',(-1.42214152323476,6.38988983122374,2.30563774552445));
#11267=CARTESIAN_POINT('Ctrl Pts',(-1.46837481356246,6.39381574245974,2.35638495257543));
#11268=CARTESIAN_POINT('Ctrl Pts',(-1.51187169559919,6.39774165369573,2.40950918440413));
#11269=CARTESIAN_POINT('Ctrl Pts',(-1.55530304717379,6.40166165032899,2.46255338163496));
#11270=CARTESIAN_POINT('Ctrl Pts',(-1.59600586540521,6.40558164696225,2.51796711955861));
#11271=CARTESIAN_POINT('Ctrl Pts',(-1.6337150448608,6.40950164359551,2.5754377750376));
#11272=CARTESIAN_POINT('Ctrl Pts',(-1.67137938712491,6.4134169792512,2.63284009641807));
#11273=CARTESIAN_POINT('Ctrl Pts',(-1.70605689353571,6.41733231490688,2.6922940697625));
#11274=CARTESIAN_POINT('Ctrl Pts',(-1.73752386585787,6.42124765056257,2.75345553548459));
#11275=CARTESIAN_POINT('Ctrl Pts',(-1.768970819619,6.42516049537214,2.81457809169476));
#11276=CARTESIAN_POINT('Ctrl Pts',(-1.79721106794491,6.42907334018171,2.87740555063099));
#11277=CARTESIAN_POINT('Ctrl Pts',(-1.82206603382122,6.43298618499128,2.94156774139191));
#11278=CARTESIAN_POINT('Ctrl Pts',(-1.84691362236179,6.4368978684084,3.00571088782885));
#11279=CARTESIAN_POINT('Ctrl Pts',(-1.86837774659705,6.44080955182552,3.07118752306012));
#11280=CARTESIAN_POINT('Ctrl Pts',(-1.88632802424344,6.44472123524263,3.13760766485144));
#11281=CARTESIAN_POINT('Ctrl Pts',(-1.90427906532718,6.44863308502627,3.20403063153597));
#11282=CARTESIAN_POINT('Ctrl Pts',(-1.91871583776213,6.45254493480991,3.27139671099792));
#11283=CARTESIAN_POINT('Ctrl Pts',(-1.92955835474803,6.45645678459355,3.33930267088887));
#11284=CARTESIAN_POINT('Ctrl Pts',(-1.94041196353363,6.46037263616518,3.40727809798073));
#11285=CARTESIAN_POINT('Ctrl Pts',(-1.94766390122193,6.46428848773681,3.47579402321349));
#11286=CARTESIAN_POINT('Ctrl Pts',(-1.95128582531457,6.46820433930844,3.54443997383869));
#11287=CARTESIAN_POINT('Ctrl Pts',(-1.95490984473786,6.47212245625163,3.61312563704788));
#11288=CARTESIAN_POINT('Ctrl Pts',(-1.95489967004011,6.47604057319483,3.68194098549075));
#11289=CARTESIAN_POINT('Ctrl Pts',(-1.95127910870616,6.47995869013802,3.75047618308775));
#11290=CARTESIAN_POINT('Ctrl Pts',(-1.94765250212591,6.48388334915571,3.81912581381036));
#11291=CARTESIAN_POINT('Ctrl Pts',(-1.94040352839182,6.4878080081734,3.88749387319111));
#11292=CARTESIAN_POINT('Ctrl Pts',(-1.92960768452086,6.49173266719108,3.95517715759252));
#11293=CARTESIAN_POINT('Ctrl Pts',(-1.92478576989575,6.49348559831367,3.98540758912072));
#11294=CARTESIAN_POINT('Ctrl Pts',(-1.91925696002774,6.49523852943625,4.01550157306799));
#11295=CARTESIAN_POINT('Ctrl Pts',(-1.91303120504268,6.49699146055883,4.04542412613984));
#11296=CARTESIAN_POINT('Ctrl Pts',(-1.89924643361079,6.50087271751781,4.11167722407641));
#11297=CARTESIAN_POINT('Ctrl Pts',(-1.88198628894891,6.50475397447679,4.17735458711253));
#11298=CARTESIAN_POINT('Ctrl Pts',(-1.86131381314334,6.50863523143576,4.24205982712176));
#11299=CARTESIAN_POINT('Ctrl Pts',(-1.84067596241916,6.51250998753633,4.30665668997177));
#11300=CARTESIAN_POINT('Ctrl Pts',(-1.81663727951453,6.5163847436369,4.370284188447));
#11301=CARTESIAN_POINT('Ctrl Pts',(-1.78931167938921,6.52025949973747,4.43255668973964));
#11302=CARTESIAN_POINT('Ctrl Pts',(-1.76201162445679,6.52413063354278,4.49477097591349));
#11303=CARTESIAN_POINT('Ctrl Pts',(-1.7314309429528,6.52800176734808,4.55563231808264));
#11304=CARTESIAN_POINT('Ctrl Pts',(-1.69773268329178,6.53187290115338,4.61477223114742));
#11305=CARTESIAN_POINT('Ctrl Pts',(-1.66405383217142,6.53574180537595,4.67387808253014));
#11306=CARTESIAN_POINT('Ctrl Pts',(-1.62726121136195,6.53961070959853,4.73126403542487));
#11307=CARTESIAN_POINT('Ctrl Pts',(-1.58756426082807,6.5434796138211,4.78658528537354));
#11308=CARTESIAN_POINT('Ctrl Pts',(-1.54787592827796,6.54734767812641,4.84189452539128));
#11309=CARTESIAN_POINT('Ctrl Pts',(-1.50528481066995,6.55121574243173,4.89513954481632));
#11310=CARTESIAN_POINT('Ctrl Pts',(-1.46004311123215,6.55508380673704,4.9460053081214));
#11311=CARTESIAN_POINT('Ctrl Pts',(-1.41476494890701,6.55895498853782,4.99691206707033));
#11312=CARTESIAN_POINT('Ctrl Pts',(-1.36683226981971,6.56282617033861,5.04543536161551));
#11313=CARTESIAN_POINT('Ctrl Pts',(-1.3165361887834,6.56669735213939,5.09129490239409));
#11314=CARTESIAN_POINT('Ctrl Pts',(-1.26622087358059,6.57057001435284,5.13717198072281));
#11315=CARTESIAN_POINT('Ctrl Pts',(-1.21354074412195,6.57444267656628,5.18038295628708));
#11316=CARTESIAN_POINT('Ctrl Pts',(-1.15882003527184,6.57831533877973,5.22068786935456));
#11317=CARTESIAN_POINT('Ctrl Pts',(-1.10400413035419,6.58219473815396,5.26106289973789));
#11318=CARTESIAN_POINT('Ctrl Pts',(-1.04714097458841,6.58607413752819,5.29852149120498));
#11319=CARTESIAN_POINT('Ctrl Pts',(-0.988583156110888,6.58995353690241,
5.33286750083403));
#11320=CARTESIAN_POINT('Ctrl Pts',(-0.938241345921017,6.59328863359873,
5.36239456216384));
#11321=CARTESIAN_POINT('Ctrl Pts',(-0.886647658348861,6.59662373029505,
5.38962186526928));
#11322=CARTESIAN_POINT('Ctrl Pts',(-0.834037993952278,6.59995882699137,
5.41445321791391));
#11323=CARTESIAN_POINT('',(-1.90834530359594,6.6,4.06731613031539));
#11324=CARTESIAN_POINT('Origin',(-1.46549439250521E-15,6.6,3.64739446828387));
#11325=CARTESIAN_POINT('Ctrl Pts',(-1.90834530359594,6.6,4.06731613031539));
#11326=CARTESIAN_POINT('Ctrl Pts',(-2.04784060254395,6.56299081980964,3.43337598697229));
#11327=CARTESIAN_POINT('Ctrl Pts',(-1.64305422583223,6.48897245942892,2.02647090284422));
#11328=CARTESIAN_POINT('Ctrl Pts',(0.47254091610022,6.37794491885784,1.38598473075092));
#11329=CARTESIAN_POINT('Ctrl Pts',(1.80025717638367,6.29024427840894,2.51599492455184));
#11330=CARTESIAN_POINT('Ctrl Pts',(1.9529603584434,6.23955281815039,3.40572641983012));
#11331=CARTESIAN_POINT('Ctrl Pts',(1.95156756343269,6.22587053808222,3.64631438782882));
#11332=CARTESIAN_POINT('Origin',(-2.67773308947627E-16,1.2059437743963,
3.64739446828387));
#11333=CARTESIAN_POINT('',(0.426542481555679,6.599956144719,2.15151955324975));
#11334=CARTESIAN_POINT('Ctrl Pts',(1.5554997682929,6.4559437743963,3.6465454448856));
#11335=CARTESIAN_POINT('Ctrl Pts',(1.55546406369716,6.46061116422838,3.58113088679472));
#11336=CARTESIAN_POINT('Ctrl Pts',(1.55129786300922,6.46527855406046,3.51586849460407));
#11337=CARTESIAN_POINT('Ctrl Pts',(1.54308295192937,6.46994594389254,3.45124336972736));
#11338=CARTESIAN_POINT('Ctrl Pts',(1.53480401511366,6.47464971063311,3.38611456670539));
#11339=CARTESIAN_POINT('Ctrl Pts',(1.52241313274287,6.47935347737368,3.32163325345467));
#11340=CARTESIAN_POINT('Ctrl Pts',(1.50604397351761,6.48405724411425,3.25827777649169));
#11341=CARTESIAN_POINT('Ctrl Pts',(1.4910402357253,6.48836864959578,3.20020705025716));
#11342=CARTESIAN_POINT('Ctrl Pts',(1.47269489336211,6.49268005507731,3.14308208717692));
#11343=CARTESIAN_POINT('Ctrl Pts',(1.45114591966537,6.49699146055883,3.0872554053374));
#11344=CARTESIAN_POINT('Ctrl Pts',(1.42970295788867,6.50128165573217,3.03170336737719));
#11345=CARTESIAN_POINT('Ctrl Pts',(1.40501473944521,6.50557185090551,2.97725350914402));
#11346=CARTESIAN_POINT('Ctrl Pts',(1.37722024457808,6.50986204607885,2.92431449488931));
#11347=CARTESIAN_POINT('Ctrl Pts',(1.35064705115635,6.51396372832576,2.87370164252155));
#11348=CARTESIAN_POINT('Ctrl Pts',(1.32123511808883,6.51806541057266,2.8244701800106));
#11349=CARTESIAN_POINT('Ctrl Pts',(1.28915582586842,6.52216709281957,2.77695922851613));
#11350=CARTESIAN_POINT('Ctrl Pts',(1.25710663774667,6.52626492593395,2.72949286261793));
#11351=CARTESIAN_POINT('Ctrl Pts',(1.22239534318046,6.53036275904833,2.68374424903125));
#11352=CARTESIAN_POINT('Ctrl Pts',(1.18523844654547,6.53446059216271,2.64002657380317));
#11353=CARTESIAN_POINT('Ctrl Pts',(1.14810147323584,6.53855622804132,2.59633233975415));
#11354=CARTESIAN_POINT('Ctrl Pts',(1.10852184009623,6.54265186391993,2.55466729042924));
#11355=CARTESIAN_POINT('Ctrl Pts',(1.06675701342171,6.54674749979854,2.51531243754776));
#11356=CARTESIAN_POINT('Ctrl Pts',(1.02499778330378,6.55084258685509,2.47596285828235));
#11357=CARTESIAN_POINT('Ctrl Pts',(0.981054328890205,6.55493767391165,2.4389232239911));
#11358=CARTESIAN_POINT('Ctrl Pts',(0.93522003928002,6.55903276096821,2.40443681489053));
#11359=CARTESIAN_POINT('Ctrl Pts',(0.889344673355693,6.56313151800817,2.36991949935319));
#11360=CARTESIAN_POINT('Ctrl Pts',(0.841575516606039,6.56723027504813,2.33796029461034));
#11361=CARTESIAN_POINT('Ctrl Pts',(0.792236695122553,6.57132903208809,2.30876036259954));
#11362=CARTESIAN_POINT('Ctrl Pts',(0.742871689082678,6.57542996437529,2.27954493392215));
#11363=CARTESIAN_POINT('Ctrl Pts',(0.691935833065454,6.57953089666248,2.25309193575008));
#11364=CARTESIAN_POINT('Ctrl Pts',(0.639776841899524,6.58363182894968,2.22955602806261));
#11365=CARTESIAN_POINT('Ctrl Pts',(0.58753186031973,6.58773952212041,2.20598131858089));
#11366=CARTESIAN_POINT('Ctrl Pts',(0.534060217488818,6.59184721529114,2.18533348088132));
#11367=CARTESIAN_POINT('Ctrl Pts',(0.47972703809965,6.59595490846187,2.16771807835392));
#11368=CARTESIAN_POINT('Ctrl Pts',(0.462085353070969,6.59728865388091,2.1619984538715));
#11369=CARTESIAN_POINT('Ctrl Pts',(0.444352929777355,6.59862239929996,2.15659812813977));
#11370=CARTESIAN_POINT('Ctrl Pts',(0.426542481555679,6.599956144719,2.15151955324975));
#11371=CARTESIAN_POINT('',(1.55328677638795,6.6,3.5644460487792));
#11372=CARTESIAN_POINT('Origin',(-1.46549439250521E-15,6.6,3.64739446828387));
#11373=CARTESIAN_POINT('Ctrl Pts',(1.55549999987963,6.59414638614667,3.64737511703584));
#11374=CARTESIAN_POINT('Ctrl Pts',(1.55549982783689,6.59510874546272,3.63354590681206));
#11375=CARTESIAN_POINT('Ctrl Pts',(1.55531523240308,6.59607695453386,3.61971776272614));
#11376=CARTESIAN_POINT('Ctrl Pts',(1.5545773647494,6.59802745792116,3.59207096791368));
#11377=CARTESIAN_POINT('Ctrl Pts',(1.55402412717384,6.59900966026662,3.57825363224026));
#11378=CARTESIAN_POINT('Ctrl Pts',(1.55328677638795,6.6,3.5644460487792));
#11379=CARTESIAN_POINT('Ctrl Pts',(0.684651324693825,2.26863408412604,5.04165517356951));
#11380=CARTESIAN_POINT('Ctrl Pts',(1.14788625211098,2.30564859368349,4.81419027525137));
#11381=CARTESIAN_POINT('Ctrl Pts',(1.82177976417329,2.3796722834313,3.86524735393602));
#11382=CARTESIAN_POINT('Ctrl Pts',(1.17126252580745,2.49070515336946,2.23289142025749));
#11383=CARTESIAN_POINT('Ctrl Pts',(-0.550929011373164,2.60173269394054,
1.8972621249236));
#11384=CARTESIAN_POINT('Ctrl Pts',(-1.76895437683424,2.71276023451162,3.15850697088285));
#11385=CARTESIAN_POINT('Ctrl Pts',(-1.37119925940374,2.8237877750827,4.86751886652752));
#11386=CARTESIAN_POINT('Ctrl Pts',(0.279566957660274,2.93481531565378,5.46119858728686));
#11387=CARTESIAN_POINT('Ctrl Pts',(1.67479408727594,3.04584285622485,4.3979960058981));
#11388=CARTESIAN_POINT('Ctrl Pts',(1.53990869075139,3.15687039679593,2.648854714652));
#11389=CARTESIAN_POINT('Ctrl Pts',(-0.00194110293598168,3.26789793736701,
1.81210655462338));
#11390=CARTESIAN_POINT('Ctrl Pts',(-1.5420014927779,3.37892547793809,2.65212320530051));
#11391=CARTESIAN_POINT('Ctrl Pts',(-1.67322430909778,3.48995301850917,4.40148852237912));
#11392=CARTESIAN_POINT('Ctrl Pts',(-0.275705577370856,3.60098055908025,
5.46186647902077));
#11393=CARTESIAN_POINT('Ctrl Pts',(1.37370863799142,3.71200809965133,4.86446239222593));
#11394=CARTESIAN_POINT('Ctrl Pts',(1.76803851820382,3.8230356402224,3.15508418544703));
#11395=CARTESIAN_POINT('Ctrl Pts',(0.547003778353852,3.93406318079349,1.89550562214907));
#11396=CARTESIAN_POINT('Ctrl Pts',(-1.17379929443624,4.04509072136456,2.23653514832174));
#11397=CARTESIAN_POINT('Ctrl Pts',(-1.8221637133016,4.15611826193564,3.86659322783984));
#11398=CARTESIAN_POINT('Ctrl Pts',(-0.805712675430428,4.26714580250672,
5.29638067585463));
#11399=CARTESIAN_POINT('Ctrl Pts',(0.946875698946843,4.3781733430778,5.2195760848642));
#11400=CARTESIAN_POINT('Ctrl Pts',(1.83435347884445,4.48920088364888,3.70635156641869));
#11401=CARTESIAN_POINT('Ctrl Pts',(1.04587869061767,4.60022842421995,2.13926112118895));
#11402=CARTESIAN_POINT('Ctrl Pts',(-0.698160489741093,4.71125596479103,
1.95007286504292));
#11403=CARTESIAN_POINT('Ctrl Pts',(-1.80432722111991,4.82228350536211,3.31163848029748));
#11404=CARTESIAN_POINT('Ctrl Pts',(-1.26197456066073,4.93331104593319,4.97996636915454));
#11405=CARTESIAN_POINT('Ctrl Pts',(0.433377472991916,5.04433858650427,5.43079391382108));
#11406=CARTESIAN_POINT('Ctrl Pts',(1.73277632833419,5.15536612707534,4.25222167463752));
#11407=CARTESIAN_POINT('Ctrl Pts',(1.44902630832145,5.26639366764643,2.521053045387));
#11408=CARTESIAN_POINT('Ctrl Pts',(-0.158619024761313,5.3774212082175,1.81895867888319));
#11409=CARTESIAN_POINT('Ctrl Pts',(-1.6213501498084,5.48844874878859,2.7874193626174));
#11410=CARTESIAN_POINT('Ctrl Pts',(-1.60272396252789,5.59947628935966,4.54157643737503));
#11411=CARTESIAN_POINT('Ctrl Pts',(-0.119801397977274,5.71050382993074,
5.47880049657949));
#11412=CARTESIAN_POINT('Ctrl Pts',(1.47263207300637,5.82153137050182,4.74269930283736));
#11413=CARTESIAN_POINT('Ctrl Pts',(1.71949372363033,5.9325589110729,3.00600192052272));
#11414=CARTESIAN_POINT('Ctrl Pts',(0.395546584890944,6.04358645164398,1.8550680874704));
#11415=CARTESIAN_POINT('Ctrl Pts',(-1.29018035693896,6.15461399221506,2.34215685811287));
#11416=CARTESIAN_POINT('Ctrl Pts',(-1.79638565259649,6.26564153278613,4.02087081558556));
#11417=CARTESIAN_POINT('Ctrl Pts',(-0.662790583736326,6.37666907335722,
5.36010676734267));
#11418=CARTESIAN_POINT('Ctrl Pts',(1.07933315373079,6.48769661392829,5.13104989888334));
#11419=CARTESIAN_POINT('Ctrl Pts',(1.57859588144957,6.56171497430901,4.07982280745058));
#11420=CARTESIAN_POINT('Ctrl Pts',(1.55108009138598,6.59872415449937,3.56456388988623));
#11421=CARTESIAN_POINT('Ctrl Pts',(0.743896982560042,2.34623717873851,5.1623062111741));
#11422=CARTESIAN_POINT('Ctrl Pts',(1.24721750834176,2.38325168829595,4.91515785201061));
#11423=CARTESIAN_POINT('Ctrl Pts',(1.9794257610814,2.45727537804376,3.88409904831387));
#11424=CARTESIAN_POINT('Ctrl Pts',(1.27261662587663,2.56830824798192,2.11048873057953));
#11425=CARTESIAN_POINT('Ctrl Pts',(-0.598603134739513,2.679335788553,1.74581607012819));
#11426=CARTESIAN_POINT('Ctrl Pts',(-1.92202917857765,2.79036332912407,3.11620155152352));
#11427=CARTESIAN_POINT('Ctrl Pts',(-1.48985469649849,2.90139086969515,4.97310118273044));
#11428=CARTESIAN_POINT('Ctrl Pts',(0.30375902116303,3.01241841026623,5.61815441924826));
#11429=CARTESIAN_POINT('Ctrl Pts',(1.81972081700291,3.12344595083731,4.46294860335526));
#11430=CARTESIAN_POINT('Ctrl Pts',(1.67316323966835,3.23447349140838,2.56244701707551));
#11431=CARTESIAN_POINT('Ctrl Pts',(-0.00210907445123478,3.34550103197947,
1.6532916427157));
#11432=CARTESIAN_POINT('Ctrl Pts',(-1.6754371403481,3.45652857255054,2.5659983434854));
#11433=CARTESIAN_POINT('Ctrl Pts',(-1.81801519954786,3.56755611312163,4.46674334146218));
#11434=CARTESIAN_POINT('Ctrl Pts',(-0.29956349996529,3.6785836536927,5.61888010636462));
#11435=CARTESIAN_POINT('Ctrl Pts',(1.49258122179998,3.78961119426379,4.96978021930246));
#11436=CARTESIAN_POINT('Ctrl Pts',(1.92103406698283,3.90063873483486,3.11248257857215));
#11437=CARTESIAN_POINT('Ctrl Pts',(0.594338235376008,4.01166627540594,1.7439075700396));
#11438=CARTESIAN_POINT('Ctrl Pts',(-1.27537291139066,4.12269381597701,2.11444776522171));
#11439=CARTESIAN_POINT('Ctrl Pts',(-1.97984293488608,4.2337213565481,3.88556138614897));
#11440=CARTESIAN_POINT('Ctrl Pts',(-0.875434263318064,4.34474889711917,
5.43907414500631));
#11441=CARTESIAN_POINT('Ctrl Pts',(1.02881269618661,4.45577643769026,5.35562334103673));
#11442=CARTESIAN_POINT('Ctrl Pts',(1.99308753031499,4.56680397826132,3.71145336340483));
#11443=CARTESIAN_POINT('Ctrl Pts',(1.13638281854237,4.67783151883242,2.00875622172268));
#11444=CARTESIAN_POINT('Ctrl Pts',(-0.758575150487437,4.78885905940348,
1.80319673792884));
#11445=CARTESIAN_POINT('Ctrl Pts',(-1.96046297864434,4.89988659997457,3.28258415195061));
#11446=CARTESIAN_POINT('Ctrl Pts',(-1.37117834127157,5.01091414054565,5.0952792241416));
#11447=CARTESIAN_POINT('Ctrl Pts',(0.470879384644959,5.12194168111673,5.58511870598642));
#11448=CARTESIAN_POINT('Ctrl Pts',(1.88272049670789,5.2329692216878,4.30455982756789));
#11449=CARTESIAN_POINT('Ctrl Pts',(1.57441643582957,5.34399676225888,2.42358615067044));
#11450=CARTESIAN_POINT('Ctrl Pts',(-0.172344972748464,5.45502430282995,
1.66073670909787));
#11451=CARTESIAN_POINT('Ctrl Pts',(-1.7616521587176,5.56605184340105,2.7130022264108));
#11452=CARTESIAN_POINT('Ctrl Pts',(-1.74141417185507,5.67707938397211,4.61895363230649));
#11453=CARTESIAN_POINT('Ctrl Pts',(-0.130168299172757,5.78810692454321,
5.63727949319146));
#11454=CARTESIAN_POINT('Ctrl Pts',(1.60006490313954,5.89913446511426,4.83748047559882));
#11455=CARTESIAN_POINT('Ctrl Pts',(1.86828849430994,6.01016200568537,2.95049962019548));
#11456=CARTESIAN_POINT('Ctrl Pts',(0.429774836255361,6.12118954625642,1.69997081136455));
#11457=CARTESIAN_POINT('Ctrl Pts',(-1.40182489957839,6.23221708682751,2.22920935023958));
#11458=CARTESIAN_POINT('Ctrl Pts',(-1.95183419396478,6.34324462739859,4.05318923971664));
#11459=CARTESIAN_POINT('Ctrl Pts',(-0.720144542963022,6.45427216796968,
5.50831471383087));
#11460=CARTESIAN_POINT('Ctrl Pts',(1.17273223212766,6.56529970854074,5.25943662488868));
#11461=CARTESIAN_POINT('Ctrl Pts',(1.7151981899943,6.63931806892147,4.11724258670156));
#11462=CARTESIAN_POINT('Ctrl Pts',(1.68530134694034,6.67632724911183,3.55739622375953));
#11463=CARTESIAN_POINT('Ctrl Pts',(0.803142640426261,2.42384027335096,5.28295724877869));
#11464=CARTESIAN_POINT('Ctrl Pts',(1.34654876457254,2.46085478290841,5.01612542876985));
#11465=CARTESIAN_POINT('Ctrl Pts',(2.1370717579895,2.53487847265622,3.90295074269172));
#11466=CARTESIAN_POINT('Ctrl Pts',(1.3739707259458,2.64591134259438,1.98808604090159));
#11467=CARTESIAN_POINT('Ctrl Pts',(-0.646277258105862,2.75693888316546,
1.59437001533278));
#11468=CARTESIAN_POINT('Ctrl Pts',(-2.07510398032106,2.86796642373654,3.07389613216417));
#11469=CARTESIAN_POINT('Ctrl Pts',(-1.60851013359324,2.97899396430762,5.07868349893336));
#11470=CARTESIAN_POINT('Ctrl Pts',(0.327951084665787,3.09002150487869,5.77511025120965));
#11471=CARTESIAN_POINT('Ctrl Pts',(1.96464754672989,3.20104904544978,4.52790120081243));
#11472=CARTESIAN_POINT('Ctrl Pts',(1.80641778858531,3.31207658602085,2.47603931949901));
#11473=CARTESIAN_POINT('Ctrl Pts',(-0.00227704596648566,3.42310412659194,
1.494476730808));
#11474=CARTESIAN_POINT('Ctrl Pts',(-1.8088727879183,3.53413166716301,2.47987348167028));
#11475=CARTESIAN_POINT('Ctrl Pts',(-1.96280608999794,3.64515920773409,4.53199816054525));
#11476=CARTESIAN_POINT('Ctrl Pts',(-0.323421422559725,3.75618674830517,
5.77589373370848));
#11477=CARTESIAN_POINT('Ctrl Pts',(1.61145380560854,3.86721428887625,5.07509804637899));
#11478=CARTESIAN_POINT('Ctrl Pts',(2.07402961576183,3.97824182944732,3.06988097169728));
#11479=CARTESIAN_POINT('Ctrl Pts',(0.641672692398164,4.08926937001841,1.59230951793014));
#11480=CARTESIAN_POINT('Ctrl Pts',(-1.37694652834506,4.20029691058948,1.99236038212167));
#11481=CARTESIAN_POINT('Ctrl Pts',(-2.13752215647056,4.31132445116056,3.90452954445811));
#11482=CARTESIAN_POINT('Ctrl Pts',(-0.945155851205701,4.42235199173164,
5.58176761415798));
#11483=CARTESIAN_POINT('Ctrl Pts',(1.11074969342638,4.53337953230272,5.49167059720925));
#11484=CARTESIAN_POINT('Ctrl Pts',(2.15182158178555,4.64440707287379,3.71655516039097));
#11485=CARTESIAN_POINT('Ctrl Pts',(1.22688694646707,4.75543461344488,1.8782513222564));
#11486=CARTESIAN_POINT('Ctrl Pts',(-0.81898981123378,4.86646215401595,1.65632061081476));
#11487=CARTESIAN_POINT('Ctrl Pts',(-2.11659873616878,4.97748969458703,3.25352982360373));
#11488=CARTESIAN_POINT('Ctrl Pts',(-1.4803821218824,5.08851723515811,5.21059207912866));
#11489=CARTESIAN_POINT('Ctrl Pts',(0.508381296297998,5.19954477572919,5.73944349815177));
#11490=CARTESIAN_POINT('Ctrl Pts',(2.0326646650816,5.31057231630027,4.35689798049827));
#11491=CARTESIAN_POINT('Ctrl Pts',(1.69980656333768,5.42159985687135,2.32611925595385));
#11492=CARTESIAN_POINT('Ctrl Pts',(-0.186070920735614,5.53262739744242,
1.50251473931255));
#11493=CARTESIAN_POINT('Ctrl Pts',(-1.90195416762681,5.64365493801351,2.63858509020417));
#11494=CARTESIAN_POINT('Ctrl Pts',(-1.88010438118225,5.75468247858458,4.69633082723795));
#11495=CARTESIAN_POINT('Ctrl Pts',(-0.140535200368238,5.86571001915566,
5.79575848980343));
#11496=CARTESIAN_POINT('Ctrl Pts',(1.72749773327271,5.97673755972674,4.9322616483603));
#11497=CARTESIAN_POINT('Ctrl Pts',(2.01708326498956,6.08776510029782,2.89499731986824));
#11498=CARTESIAN_POINT('Ctrl Pts',(0.464003087619777,6.19879264086889,1.54487353525871));
#11499=CARTESIAN_POINT('Ctrl Pts',(-1.51346944221782,6.30982018143997,2.1162618423663));
#11500=CARTESIAN_POINT('Ctrl Pts',(-2.10728273533306,6.42084772201105,4.08550766384771));
#11501=CARTESIAN_POINT('Ctrl Pts',(-0.777498502189718,6.53187526258214,
5.65652266031908));
#11502=CARTESIAN_POINT('Ctrl Pts',(1.26613131052453,6.64290280315321,5.38782335089402));
#11503=CARTESIAN_POINT('Ctrl Pts',(1.85180049853903,6.71692116353393,4.15466236595253));
#11504=CARTESIAN_POINT('Ctrl Pts',(1.81952260249468,6.75393034372429,3.55022855763283));
#11505=CARTESIAN_POINT('Ctrl Pts',(0.862388298292479,2.50144336796343,5.40360828638328));
#11506=CARTESIAN_POINT('Ctrl Pts',(1.44588002080332,2.53845787752087,5.11709300552908));
#11507=CARTESIAN_POINT('Ctrl Pts',(2.29471775489761,2.61248156726868,3.92180243706957));
#11508=CARTESIAN_POINT('Ctrl Pts',(1.47532482601497,2.72351443720684,1.86568335122363));
#11509=CARTESIAN_POINT('Ctrl Pts',(-0.693951381472212,2.83454197777791,
1.44292396053739));
#11510=CARTESIAN_POINT('Ctrl Pts',(-2.22817878206447,2.945569518349,3.03159071280484));
#11511=CARTESIAN_POINT('Ctrl Pts',(-1.72716557068799,3.05659705892007,5.18426581513628));
#11512=CARTESIAN_POINT('Ctrl Pts',(0.352143148168543,3.16762459949115,5.93206608317104));
#11513=CARTESIAN_POINT('Ctrl Pts',(2.10957427645686,3.27865214006223,4.5928537982696));
#11514=CARTESIAN_POINT('Ctrl Pts',(1.93967233750227,3.38967968063331,2.38963162192252));
#11515=CARTESIAN_POINT('Ctrl Pts',(-0.00244501748173502,3.50070722120439,
1.33566181890031));
#11516=CARTESIAN_POINT('Ctrl Pts',(-1.94230843548851,3.61173476177546,2.39374861985516));
#11517=CARTESIAN_POINT('Ctrl Pts',(-2.10759698044802,3.72276230234655,4.59725297962832));
#11518=CARTESIAN_POINT('Ctrl Pts',(-0.347279345154162,3.83378984291762,
5.93290736105231));
#11519=CARTESIAN_POINT('Ctrl Pts',(1.73032638941711,3.9448173834887,5.18041587345552));
#11520=CARTESIAN_POINT('Ctrl Pts',(2.22702516454082,4.05584492405978,3.0272793648224));
#11521=CARTESIAN_POINT('Ctrl Pts',(0.689007149420318,4.16687246463086,1.44071146582068));
#11522=CARTESIAN_POINT('Ctrl Pts',(-1.47852014529947,4.27790000520195,1.87027299902164));
#11523=CARTESIAN_POINT('Ctrl Pts',(-2.29520137805504,4.38892754577301,3.92349770276724));
#11524=CARTESIAN_POINT('Ctrl Pts',(-1.01487743909333,4.4999550863441,5.72446108330965));
#11525=CARTESIAN_POINT('Ctrl Pts',(1.19268669066615,4.61098262691517,5.62771785338177));
#11526=CARTESIAN_POINT('Ctrl Pts',(2.31055563325609,4.72201016748625,3.72165695737712));
#11527=CARTESIAN_POINT('Ctrl Pts',(1.31739107439176,4.83303770805733,1.74774642279012));
#11528=CARTESIAN_POINT('Ctrl Pts',(-0.879404471980124,4.94406524862841,
1.50944448370067));
#11529=CARTESIAN_POINT('Ctrl Pts',(-2.2727344936932,5.05509278919948,3.22447549525686));
#11530=CARTESIAN_POINT('Ctrl Pts',(-1.58958590249323,5.16612032977057,5.32590493411573));
#11531=CARTESIAN_POINT('Ctrl Pts',(0.545883207951039,5.27714787034165,5.8937682903171));
#11532=CARTESIAN_POINT('Ctrl Pts',(2.1826088334553,5.38817541091274,4.40923613342865));
#11533=CARTESIAN_POINT('Ctrl Pts',(1.8251966908458,5.49920295148381,2.22865236123728));
#11534=CARTESIAN_POINT('Ctrl Pts',(-0.199796868722764,5.61023049205489,
1.34429276952724));
#11535=CARTESIAN_POINT('Ctrl Pts',(-2.04225617653602,5.72125803262598,2.56416795399757));
#11536=CARTESIAN_POINT('Ctrl Pts',(-2.01879459050944,5.83228557319703,4.77370802216941));
#11537=CARTESIAN_POINT('Ctrl Pts',(-0.15090210156372,5.94331311376812,5.95423748641541));
#11538=CARTESIAN_POINT('Ctrl Pts',(1.85493056340587,6.0543406543392,5.02704282112175));
#11539=CARTESIAN_POINT('Ctrl Pts',(2.16587803566918,6.16536819491026,2.83949501954101));
#11540=CARTESIAN_POINT('Ctrl Pts',(0.498231338984191,6.27639573548136,1.38977625915286));
#11541=CARTESIAN_POINT('Ctrl Pts',(-1.62511398485724,6.38742327605242,2.00331433449301));
#11542=CARTESIAN_POINT('Ctrl Pts',(-2.26273127670134,6.49845081662351,4.1178260879788));
#11543=CARTESIAN_POINT('Ctrl Pts',(-0.834852461416417,6.60947835719459,
5.80473060680729));
#11544=CARTESIAN_POINT('Ctrl Pts',(1.3595303889214,6.72050589776568,5.51621007689934));
#11545=CARTESIAN_POINT('Ctrl Pts',(1.98840280708377,6.79452425814639,4.1920821452035));
#11546=CARTESIAN_POINT('Ctrl Pts',(1.95374385804904,6.83153343833676,3.54306089150614));
#11547=CARTESIAN_POINT('Ctrl Pts',(-0.83475068776765,6.6,5.41764852956582));
#11548=CARTESIAN_POINT('Ctrl Pts',(-0.7907192463387,6.6,5.43356975418934));
#11549=CARTESIAN_POINT('Ctrl Pts',(-0.746172855022355,6.6,5.44776191297247));
#11550=CARTESIAN_POINT('Ctrl Pts',(-0.701168580024064,6.6,5.46015373566206));
#11551=CARTESIAN_POINT('Ctrl Pts',(-0.632780325123476,6.6,5.47898428295588));
#11552=CARTESIAN_POINT('Ctrl Pts',(-0.563334570914971,6.6,5.49366007719785));
#11553=CARTESIAN_POINT('Ctrl Pts',(-0.49318299999272,6.6,5.50428783506038));
#11554=CARTESIAN_POINT('Ctrl Pts',(-0.422101207184304,6.6,5.51505651881859));
#11555=CARTESIAN_POINT('Ctrl Pts',(-0.350293636793303,6.6,5.52166884246449));
#11556=CARTESIAN_POINT('Ctrl Pts',(-0.278132525181492,6.6,5.52418340588826));
#11557=CARTESIAN_POINT('Ctrl Pts',(-0.245886653883812,6.6,5.52530706220011));
#11558=CARTESIAN_POINT('Ctrl Pts',(-0.213570373240598,6.6,5.52561179547267));
#11559=CARTESIAN_POINT('Ctrl Pts',(-0.181218209318684,6.6,5.52509972733527));
#11560=CARTESIAN_POINT('Ctrl Pts',(-0.160635756765334,6.6,5.5247739494934));
#11561=CARTESIAN_POINT('Ctrl Pts',(-0.140038799820486,6.6,5.52411753323216));
#11562=CARTESIAN_POINT('Ctrl Pts',(-0.119436477969568,6.6,5.52313064631106));
#11563=CARTESIAN_POINT('Ctrl Pts',(-0.107012385205877,6.6,5.52253551073635));
#11564=CARTESIAN_POINT('Ctrl Pts',(-0.0945852684134668,6.6,5.52182002861019));
#11565=CARTESIAN_POINT('Ctrl Pts',(-0.0821742362766652,6.6,5.52098560168541));
#11566=CARTESIAN_POINT('Ctrl Pts',(-0.0118828483446975,6.6,5.51625972344871));
#11567=CARTESIAN_POINT('Ctrl Pts',(0.0580208766311918,6.6,5.50771766688765));
#11568=CARTESIAN_POINT('Ctrl Pts',(0.127194914653329,6.6,5.49545172311723));
#11569=CARTESIAN_POINT('Ctrl Pts',(0.195407928457269,6.6,5.4833561882077));
#11570=CARTESIAN_POINT('Ctrl Pts',(0.262912350191099,6.6,5.46763903161575));
#11571=CARTESIAN_POINT('Ctrl Pts',(0.329361205535183,6.6,5.44834294016202));
#11572=CARTESIAN_POINT('Ctrl Pts',(0.394438685628238,6.6,5.42944508253977));
#11573=CARTESIAN_POINT('Ctrl Pts',(0.458504499769621,6.6,5.40711402878233));
#11574=CARTESIAN_POINT('Ctrl Pts',(0.521201674006322,6.6,5.38135263368176));
#11575=CARTESIAN_POINT('Ctrl Pts',(0.536341223462779,6.6,5.37513200380584));
#11576=CARTESIAN_POINT('Ctrl Pts',(0.551400795453242,6.6,5.3687112007047));
#11577=CARTESIAN_POINT('Ctrl Pts',(0.566375007947456,6.6,5.3620899749367));
#11578=CARTESIAN_POINT('Ctrl Pts',(0.580397210890301,6.6,5.3558897042056));
#11579=CARTESIAN_POINT('Ctrl Pts',(0.594348562080344,6.6,5.34951165292926));
#11580=CARTESIAN_POINT('Ctrl Pts',(0.608198751045081,6.6,5.34296812914597));
#11581=CARTESIAN_POINT('Ctrl Pts',(0.668835467698714,6.6,5.31432030357665));
#11582=CARTESIAN_POINT('Ctrl Pts',(0.727626283796037,6.6,5.28246636804899));
#11583=CARTESIAN_POINT('Ctrl Pts',(0.784252300197534,6.6,5.24745318934579));
#11584=CARTESIAN_POINT('Ctrl Pts',(0.839181586975068,6.6,5.21348913790441));
#11585=CARTESIAN_POINT('Ctrl Pts',(0.892074481299448,6.6,5.17655181654566));
#11586=CARTESIAN_POINT('Ctrl Pts',(0.942605638187179,6.6,5.13664980587656));
#11587=CARTESIAN_POINT('Ctrl Pts',(0.971967892807195,6.6,5.11346385350029));
#11588=CARTESIAN_POINT('Ctrl Pts',(1.00053202791341,6.6,5.08927628734268));
#11589=CARTESIAN_POINT('Ctrl Pts',(1.0282274369325,6.6,5.06408422531173));
#11590=CARTESIAN_POINT('Ctrl Pts',(1.05360839269705,6.6,5.0409974165347));
#11591=CARTESIAN_POINT('Ctrl Pts',(1.0782596465578,6.6,5.01706684049449));
#11592=CARTESIAN_POINT('Ctrl Pts',(1.10215906011826,6.6,4.99233467734654));
#11593=CARTESIAN_POINT('Ctrl Pts',(1.11213104592551,6.6,4.9820152283245));
#11594=CARTESIAN_POINT('Ctrl Pts',(1.12197209809735,6.6,4.97155621627406));
#11595=CARTESIAN_POINT('Ctrl Pts',(1.13168042859955,6.6,4.96096067325043));
#11596=CARTESIAN_POINT('Ctrl Pts',(1.13846377674299,6.6,4.95355741714148));
#11597=CARTESIAN_POINT('Ctrl Pts',(1.14518055018692,6.6,4.94608936910646));
#11598=CARTESIAN_POINT('Ctrl Pts',(1.15182470138071,6.6,4.93856413487155));
#11599=CARTESIAN_POINT('Ctrl Pts',(1.1947391474218,6.6,4.8899587902457));
#11600=CARTESIAN_POINT('Ctrl Pts',(1.23469798287611,6.6,4.8388936680893));
#11601=CARTESIAN_POINT('Ctrl Pts',(1.27161691603853,6.6,4.78569376463853));
#11602=CARTESIAN_POINT('Ctrl Pts',(1.30884832136374,6.6,4.73204359116456));
#11603=CARTESIAN_POINT('Ctrl Pts',(1.3429884558849,6.6,4.67622123940713));
#11604=CARTESIAN_POINT('Ctrl Pts',(1.37390225448353,6.6,4.61854045655832));
#11605=CARTESIAN_POINT('Ctrl Pts',(1.39543358779238,6.6,4.57836602904272));
#11606=CARTESIAN_POINT('Ctrl Pts',(1.41539879061861,6.6,4.53728964580654));
#11607=CARTESIAN_POINT('Ctrl Pts',(1.4337373029043,6.6,4.49541608766621));
#11608=CARTESIAN_POINT('Ctrl Pts',(1.44483372946547,6.6,4.47007887080145));
#11609=CARTESIAN_POINT('Ctrl Pts',(1.45533433091002,6.6,4.44444978212132));
#11610=CARTESIAN_POINT('Ctrl Pts',(1.46522340816155,6.6,4.41855234498481));
#11611=CARTESIAN_POINT('Ctrl Pts',(1.47071187773358,6.6,4.4041791843651));
#11612=CARTESIAN_POINT('Ctrl Pts',(1.47601290065572,6.6,4.3897202501464));
#11613=CARTESIAN_POINT('Ctrl Pts',(1.48111560166178,6.6,4.37520350423181));
#11614=CARTESIAN_POINT('Ctrl Pts',(1.50212938442664,6.6,4.31542109786712));
#11615=CARTESIAN_POINT('Ctrl Pts',(1.51981558387626,6.6,4.25457930080361));
#11616=CARTESIAN_POINT('Ctrl Pts',(1.53403760689704,6.6,4.19297054210301));
#11617=CARTESIAN_POINT('Ctrl Pts',(1.54599109479687,6.6,4.14118891085586));
#11618=CARTESIAN_POINT('Ctrl Pts',(1.55549659766993,6.6,4.08886504394274));
#11619=CARTESIAN_POINT('Ctrl Pts',(1.562444707927,6.6,4.03617640078462));
#11620=CARTESIAN_POINT('Ctrl Pts',(1.56482594200129,6.6,4.01811911790135));
#11621=CARTESIAN_POINT('Ctrl Pts',(1.56690656933101,6.6,4.00001905247287));
#11622=CARTESIAN_POINT('Ctrl Pts',(1.56868146279202,6.6,3.98188358852107));
#11623=CARTESIAN_POINT('Ctrl Pts',(1.56996504112484,6.6,3.96876827253417));
#11624=CARTESIAN_POINT('Ctrl Pts',(1.57108783615978,6.6,3.95564316680129));
#11625=CARTESIAN_POINT('Ctrl Pts',(1.57204829872014,6.6,3.94251393050095));
#11626=CARTESIAN_POINT('Ctrl Pts',(1.57651492193268,6.6,3.8814565254104));
#11627=CARTESIAN_POINT('Ctrl Pts',(1.5774768860156,6.6,3.82028786924348));
#11628=CARTESIAN_POINT('Ctrl Pts',(1.57477701172009,6.6,3.75928439561325));
#11629=CARTESIAN_POINT('Ctrl Pts',(1.57207713742458,6.6,3.69828092198303));
#11630=CARTESIAN_POINT('Ctrl Pts',(1.5657155359986,6.6,3.63744172301404));
#11631=CARTESIAN_POINT('Ctrl Pts',(1.55548296576947,6.6,3.57706412384393));
#11632=CARTESIAN_POINT('Ctrl Pts',(1.55476975631434,6.6,3.57285580925216));
#11633=CARTESIAN_POINT('Ctrl Pts',(1.55403772001654,6.6,3.56864974882339));
#11634=CARTESIAN_POINT('Ctrl Pts',(1.55328677638795,6.6,3.5644460487792));
#11635=CARTESIAN_POINT('Ctrl Pts',(0.905551381329051,2.5,2.37953274318763));
#11636=CARTESIAN_POINT('Ctrl Pts',(0.93880750735117,2.5,2.39730741392822));
#11637=CARTESIAN_POINT('Ctrl Pts',(0.971294169096419,2.5,2.41632950410138));
#11638=CARTESIAN_POINT('Ctrl Pts',(1.00293325234873,2.5,2.43657864884141));
#11639=CARTESIAN_POINT('Ctrl Pts',(1.05261738259362,2.5,2.46837669863281));
#11640=CARTESIAN_POINT('Ctrl Pts',(1.10021262907751,2.5,2.50319771185004));
#11641=CARTESIAN_POINT('Ctrl Pts',(1.14565012573383,2.5,2.54071161219957));
#11642=CARTESIAN_POINT('Ctrl Pts',(1.19258297319328,2.5,2.57946009731157));
#11643=CARTESIAN_POINT('Ctrl Pts',(1.23721436530706,2.5,2.62108203509865));
#11644=CARTESIAN_POINT('Ctrl Pts',(1.27944920585672,2.5,2.66526593419356));
#11645=CARTESIAN_POINT('Ctrl Pts',(1.29885420450408,2.5,2.68556643707253));
#11646=CARTESIAN_POINT('Ctrl Pts',(1.3177529711192,2.5,2.70640843912578));
#11647=CARTESIAN_POINT('Ctrl Pts',(1.33613438528024,2.5,2.7277648485129));
#11648=CARTESIAN_POINT('Ctrl Pts',(1.34511395963642,2.5,2.73819774907173));
#11649=CARTESIAN_POINT('Ctrl Pts',(1.35397004983125,2.5,2.7487534378361));
#11650=CARTESIAN_POINT('Ctrl Pts',(1.36270123656557,2.5,2.75942890284171));
#11651=CARTESIAN_POINT('Ctrl Pts',(1.37087012055007,2.5,2.76941685038711));
#11652=CARTESIAN_POINT('Ctrl Pts',(1.37893068791712,2.5,2.77951115669149));
#11653=CARTESIAN_POINT('Ctrl Pts',(1.38686853165449,2.5,2.78969190446717));
#11654=CARTESIAN_POINT('Ctrl Pts',(1.42575294049156,2.5,2.83956342775162));
#11655=CARTESIAN_POINT('Ctrl Pts',(1.4617682837703,2.5,2.89159377975069));
#11656=CARTESIAN_POINT('Ctrl Pts',(1.49483280836886,2.5,2.94542719131568));
#11657=CARTESIAN_POINT('Ctrl Pts',(1.52879779254209,2.5,3.00072666995616));
#11658=CARTESIAN_POINT('Ctrl Pts',(1.55964980037441,2.5,3.05792940973309));
#11659=CARTESIAN_POINT('Ctrl Pts',(1.58727136569837,2.5,3.11669729836776));
#11660=CARTESIAN_POINT('Ctrl Pts',(1.61427745983468,2.5,3.17415570501651));
#11661=CARTESIAN_POINT('Ctrl Pts',(1.63819595312473,2.5,3.2331112717908));
#11662=CARTESIAN_POINT('Ctrl Pts',(1.65888103081932,2.5,3.29327996688395));
#11663=CARTESIAN_POINT('Ctrl Pts',(1.66330526486009,2.5,3.30614916626286));
#11664=CARTESIAN_POINT('Ctrl Pts',(1.66758143128018,2.5,3.3190739507735));
#11665=CARTESIAN_POINT('Ctrl Pts',(1.67170785004731,2.5,3.3320516709478));
#11666=CARTESIAN_POINT('Ctrl Pts',(1.67470502407642,2.5,3.34147787998246));
#11667=CARTESIAN_POINT('Ctrl Pts',(1.67762270870614,2.5,3.3509306725004));
#11668=CARTESIAN_POINT('Ctrl Pts',(1.68045765017757,2.5,3.36039960222491));
#11669=CARTESIAN_POINT('Ctrl Pts',(1.69969107442491,2.5,3.42464076712906));
#11670=CARTESIAN_POINT('Ctrl Pts',(1.71515655755157,2.5,3.48973852400943));
#11671=CARTESIAN_POINT('Ctrl Pts',(1.72674329034789,2.5,3.5553343327368));
#11672=CARTESIAN_POINT('Ctrl Pts',(1.73830533427205,2.5,3.62079037069669));
#11673=CARTESIAN_POINT('Ctrl Pts',(1.74600577016182,2.5,3.68674333666893));
#11674=CARTESIAN_POINT('Ctrl Pts',(1.74969313315442,2.5,3.75286685206911));
#11675=CARTESIAN_POINT('Ctrl Pts',(1.75158782641231,2.5,3.78684337650342));
#11676=CARTESIAN_POINT('Ctrl Pts',(1.75242223721543,2.5,3.82086532261504));
#11677=CARTESIAN_POINT('Ctrl Pts',(1.75217071705448,2.5,3.85489016933049));
#11678=CARTESIAN_POINT('Ctrl Pts',(1.75188640575889,2.5,3.89335089635671));
#11679=CARTESIAN_POINT('Ctrl Pts',(1.75021469129045,2.5,3.93181536987594));
#11680=CARTESIAN_POINT('Ctrl Pts',(1.74719268051567,2.5,3.97023541010561));
#11681=CARTESIAN_POINT('Ctrl Pts',(1.74626233628355,2.5,3.98206325106621));
#11682=CARTESIAN_POINT('Ctrl Pts',(1.74520379369109,2.5,3.99388863698127));
#11683=CARTESIAN_POINT('Ctrl Pts',(1.74401857389663,2.5,4.00570464319947));
#11684=CARTESIAN_POINT('Ctrl Pts',(1.73748874453672,2.5,4.07080354272976));
#11685=CARTESIAN_POINT('Ctrl Pts',(1.72714356193382,2.5,4.13537383510635));
#11686=CARTESIAN_POINT('Ctrl Pts',(1.71324196470453,2.5,4.19917345782921));
#11687=CARTESIAN_POINT('Ctrl Pts',(1.69886014349002,2.5,4.26517700781126));
#11688=CARTESIAN_POINT('Ctrl Pts',(1.68067195249187,2.5,4.33035647617853));
#11689=CARTESIAN_POINT('Ctrl Pts',(1.65890851542243,2.5,4.39445447707118));
#11690=CARTESIAN_POINT('Ctrl Pts',(1.64157193770915,2.5,4.44551442546975));
#11691=CARTESIAN_POINT('Ctrl Pts',(1.62196549958368,2.5,4.49588849772744));
#11692=CARTESIAN_POINT('Ctrl Pts',(1.60018245343868,2.5,4.54544604562494));
#11693=CARTESIAN_POINT('Ctrl Pts',(1.58725007186591,2.5,4.57486787739977));
#11694=CARTESIAN_POINT('Ctrl Pts',(1.57355011774653,2.5,4.60400187538072));
#11695=CARTESIAN_POINT('Ctrl Pts',(1.55909887661838,2.5,4.63281994275618));
#11696=CARTESIAN_POINT('Ctrl Pts',(1.55322527455423,2.5,4.64453283706888));
#11697=CARTESIAN_POINT('Ctrl Pts',(1.54722753643038,2.5,4.65619353196182));
#11698=CARTESIAN_POINT('Ctrl Pts',(1.54110664803519,2.5,4.66780009865119));
#11699=CARTESIAN_POINT('Ctrl Pts',(1.53534542548472,2.5,4.67872465885014));
#11700=CARTESIAN_POINT('Ctrl Pts',(1.52947966959677,2.5,4.68959258354897));
#11701=CARTESIAN_POINT('Ctrl Pts',(1.52351124624247,2.5,4.70040147770194));
#11702=CARTESIAN_POINT('Ctrl Pts',(1.48912287727678,2.5,4.7626792717152));
#11703=CARTESIAN_POINT('Ctrl Pts',(1.45132521312236,2.5,4.82300799805288));
#11704=CARTESIAN_POINT('Ctrl Pts',(1.41034991342183,2.5,4.88110430170117));
#11705=CARTESIAN_POINT('Ctrl Pts',(1.37394992446206,2.5,4.93271355964086));
#11706=CARTESIAN_POINT('Ctrl Pts',(1.33504133707781,2.5,4.98256157219523));
#11707=CARTESIAN_POINT('Ctrl Pts',(1.29375331928111,2.5,5.03044054308138));
#11708=CARTESIAN_POINT('Ctrl Pts',(1.28165188884384,2.5,5.04447376788862));
#11709=CARTESIAN_POINT('Ctrl Pts',(1.26934585903873,2.5,5.05833775129039));
#11710=CARTESIAN_POINT('Ctrl Pts',(1.25683802025374,2.5,5.0720270093414));
#11711=CARTESIAN_POINT('Ctrl Pts',(1.24131610083745,2.5,5.08901504092617));
#11712=CARTESIAN_POINT('Ctrl Pts',(1.22549768695784,2.5,5.10571818778577));
#11713=CARTESIAN_POINT('Ctrl Pts',(1.2093967828829,2.5,5.12212019708054));
#11714=CARTESIAN_POINT('Ctrl Pts',(1.15862553679579,2.5,5.17384092321813));
#11715=CARTESIAN_POINT('Ctrl Pts',(1.1050280730408,2.5,5.2225917566086));
#11716=CARTESIAN_POINT('Ctrl Pts',(1.04880818331837,2.5,5.26807455143759));
#11717=CARTESIAN_POINT('Ctrl Pts',(0.999177416468837,2.5,5.30822663990606));
#11718=CARTESIAN_POINT('Ctrl Pts',(0.947501993564268,2.5,5.34583208873346));
#11719=CARTESIAN_POINT('Ctrl Pts',(0.893894163889863,2.5,5.38066677880411));
#11720=CARTESIAN_POINT('Ctrl Pts',(0.883181709025403,2.5,5.38762779638989));
#11721=CARTESIAN_POINT('Ctrl Pts',(0.872392012801787,2.5,5.39447809859823));
#11722=CARTESIAN_POINT('Ctrl Pts',(0.86152585967053,2.5,5.40121577991141));
#11723=CARTESIAN_POINT('Ctrl Pts',(-1.13599383904839,2.2684956023837,2.05457297837212));
#11724=CARTESIAN_POINT('Ctrl Pts',(-1.66530114882627,2.30551665559472,2.43205274651924));
#11725=CARTESIAN_POINT('Ctrl Pts',(-2.30874613777931,2.37954688899609,3.74944295559739));
#11726=CARTESIAN_POINT('Ctrl Pts',(-1.16608200062918,2.49058630258783,5.64507475471972));
#11727=CARTESIAN_POINT('Ctrl Pts',(1.04293058450782,2.60161384315891,5.70965731572961));
#11728=CARTESIAN_POINT('Ctrl Pts',(2.2985040575111,2.71264138372999,3.89288000979708));
#11729=CARTESIAN_POINT('Ctrl Pts',(1.45435102275404,2.82366892430106,1.85036189287024));
#11730=CARTESIAN_POINT('Ctrl Pts',(-0.718720235097675,2.93469646487215,
1.4504525726535));
#11731=CARTESIAN_POINT('Ctrl Pts',(-2.23505443062616,3.04572400544322,3.05738160024003));
#11732=CARTESIAN_POINT('Ctrl Pts',(-1.70937833319428,3.15675154601431,5.20357835530822));
#11733=CARTESIAN_POINT('Ctrl Pts',(0.378088709672631,3.26777908658538,5.92786550335696));
#11734=CARTESIAN_POINT('Ctrl Pts',(2.12010467341403,3.37880662715646,4.56866108547329));
#11735=CARTESIAN_POINT('Ctrl Pts',(1.92509810864168,3.48983416772754,2.36771502264023));
#11736=CARTESIAN_POINT('Ctrl Pts',(-0.0287726246970399,3.60086170829862,
1.3359598329503));
#11737=CARTESIAN_POINT('Ctrl Pts',(-1.95635373610663,3.71188924886969,2.41603341962473));
#11738=CARTESIAN_POINT('Ctrl Pts',(-2.0965179233959,3.82291678944078,4.62114101481739));
#11739=CARTESIAN_POINT('Ctrl Pts',(-0.321203270128677,3.93394433001185,
5.93658538901197));
#11740=CARTESIAN_POINT('Ctrl Pts',(1.74757773142461,4.04497187058293,5.16051723839122));
#11741=CARTESIAN_POINT('Ctrl Pts',(2.2196887832987,4.15599941115401,3.00198764182795));
#11742=CARTESIAN_POINT('Ctrl Pts',(0.663786606567354,4.26702695172509,1.43313269957975));
#11743=CARTESIAN_POINT('Ctrl Pts',(-1.49858251767498,4.37805449229617,1.88733236901576));
#11744=CARTESIAN_POINT('Ctrl Pts',(-2.29177547185453,4.48908203286725,3.949608535076));
#11745=CARTESIAN_POINT('Ctrl Pts',(-0.991093389100879,4.60010957343832,
5.73576745544));
#11746=CARTESIAN_POINT('Ctrl Pts',(1.21509863142361,4.7111371140094,5.61388972183788));
#11747=CARTESIAN_POINT('Ctrl Pts',(2.31111895030389,4.82216465458049,3.69532819685544));
#11748=CARTESIAN_POINT('Ctrl Pts',(1.29559086556015,4.93319219515156,1.73297264398224));
#11749=CARTESIAN_POINT('Ctrl Pts',(-0.903650040337952,5.04421973572264,
1.51972289010189));
#11750=CARTESIAN_POINT('Ctrl Pts',(-2.27727441159882,5.15524727629372,3.25041685278073));
#11751=CARTESIAN_POINT('Ctrl Pts',(-1.57027056200704,5.26627481686479,5.34380488426395));
#11752=CARTESIAN_POINT('Ctrl Pts',(0.571403078011824,5.37730235743588,5.88727855768163));
#11753=CARTESIAN_POINT('Ctrl Pts',(2.19102344350068,5.48832989800695,4.38427456450717));
#11754=CARTESIAN_POINT('Ctrl Pts',(1.80880579267535,5.59935743857804,2.20804710973091));
#11755=CARTESIAN_POINT('Ctrl Pts',(-0.225994198385466,5.71038497914911,
1.34682732113855));
#11756=CARTESIAN_POINT('Ctrl Pts',(-2.05437013573578,5.82141251972019,2.5876082456352));
#11757=CARTESIAN_POINT('Ctrl Pts',(-2.00567014672563,5.93244006029126,4.79648094529437));
#11758=CARTESIAN_POINT('Ctrl Pts',(-0.124697940094913,6.04346760086235,
5.95583840267334));
#11759=CARTESIAN_POINT('Ctrl Pts',(1.87059546628155,6.15449514143342,5.00542858236713));
#11760=CARTESIAN_POINT('Ctrl Pts',(2.15606965103839,6.2655226820045,2.81553154933147));
#11761=CARTESIAN_POINT('Ctrl Pts',(0.473125107460961,6.37655022257559,1.3831890024094));
#11762=CARTESIAN_POINT('Ctrl Pts',(-1.64508549561477,6.48757776314665,2.02446699268324));
#11763=CARTESIAN_POINT('Ctrl Pts',(-2.0503723003236,6.56159612352738,3.43311140089402));
#11764=CARTESIAN_POINT('Ctrl Pts',(-1.91070454657702,6.59860530371774,4.06783526971427));
#11765=CARTESIAN_POINT('Ctrl Pts',(-1.05786062916686,2.34618472182287,2.16412661457789));
#11766=CARTESIAN_POINT('Ctrl Pts',(-1.55076239015994,2.38320577503389,2.51564347259569));
#11767=CARTESIAN_POINT('Ctrl Pts',(-2.14995148560286,2.45723600843527,3.74242410073808));
#11768=CARTESIAN_POINT('Ctrl Pts',(-1.08587933881672,2.568275422027,5.50767508957099));
#11769=CARTESIAN_POINT('Ctrl Pts',(0.971198228706071,2.67930296259808,5.56781568741114));
#11770=CARTESIAN_POINT('Ctrl Pts',(2.14041385159104,2.79033050316915,3.87599561071092));
#11771=CARTESIAN_POINT('Ctrl Pts',(1.35432133086994,2.90135804374023,1.97396108729576));
#11772=CARTESIAN_POINT('Ctrl Pts',(-0.669286939735767,3.01238558431131,
1.60155737298641));
#11773=CARTESIAN_POINT('Ctrl Pts',(-2.08132826511188,3.12341312488239,3.0979624534692));
#11774=CARTESIAN_POINT('Ctrl Pts',(-1.59180796310647,3.23444066545347,5.09654463903298));
#11775=CARTESIAN_POINT('Ctrl Pts',(0.352083916784465,3.34546820602455,5.77101560163446));
#11776=CARTESIAN_POINT('Ctrl Pts',(1.97428470703338,3.45649574659562,4.50529672953804));
#11777=CARTESIAN_POINT('Ctrl Pts',(1.79269061716177,3.56752328716671,2.45573087208473));
#11778=CARTESIAN_POINT('Ctrl Pts',(-0.0267936548760603,3.67855082773777,
1.49493939893213));
#11779=CARTESIAN_POINT('Ctrl Pts',(-1.82179649485102,3.78957836830887,2.50072594871048));
#11780=CARTESIAN_POINT('Ctrl Pts',(-1.9523202444135,3.90060590887993,4.55416710996289));
#11781=CARTESIAN_POINT('Ctrl Pts',(-0.299111035420236,4.01163344945102,
5.77913573698044));
#11782=CARTESIAN_POINT('Ctrl Pts',(1.62738002173627,4.12266099002209,5.05644524881745));
#11783=CARTESIAN_POINT('Ctrl Pts',(2.06701946096995,4.23368853059318,3.04637846975065));
#11784=CARTESIAN_POINT('Ctrl Pts',(0.618131624590583,4.34471607116425,1.58542875397713));
#11785=CARTESIAN_POINT('Ctrl Pts',(-1.39551060095016,4.45574361173534,2.00838874861888));
#11786=CARTESIAN_POINT('Ctrl Pts',(-2.13414805541208,4.56677115230641,3.92882237031159));
#11787=CARTESIAN_POINT('Ctrl Pts',(-0.922926375230729,4.67779869287749,
5.59212998197178));
#11788=CARTESIAN_POINT('Ctrl Pts',(1.13152462500531,4.78882623344857,5.47863495099715));
#11789=CARTESIAN_POINT('Ctrl Pts',(2.15216109701436,4.89985377401965,3.69203133383899));
#11790=CARTESIAN_POINT('Ctrl Pts',(1.20648063490589,5.01088131459073,1.86464582482029));
#11791=CARTESIAN_POINT('Ctrl Pts',(-0.841497345636436,5.1219088551618,1.66606330521921));
#11792=CARTESIAN_POINT('Ctrl Pts',(-2.12064437238283,5.23293639573289,3.27772081718985));
#11793=CARTESIAN_POINT('Ctrl Pts',(-1.46226796976159,5.34396393630395,5.22712644242662));
#11794=CARTESIAN_POINT('Ctrl Pts',(0.532102198828668,5.45499147687504,5.73322021013476));
#11795=CARTESIAN_POINT('Ctrl Pts',(2.04032571197971,5.56601901744612,4.33359224103263));
#11796=CARTESIAN_POINT('Ctrl Pts',(1.68439684099264,5.6770465580172,2.30704485548669));
#11797=CARTESIAN_POINT('Ctrl Pts',(-0.210450406220845,5.78807409858828,
1.50505942555297));
#11798=CARTESIAN_POINT('Ctrl Pts',(-1.91307136502743,5.89910163915935,2.66049992560517));
#11799=CARTESIAN_POINT('Ctrl Pts',(-1.86772094212563,6.01012917973043,4.71744722891832));
#11800=CARTESIAN_POINT('Ctrl Pts',(-0.116121264772982,6.12115672030151,
5.79706453592731));
#11801=CARTESIAN_POINT('Ctrl Pts',(1.74193664512734,6.23218426087259,4.9120235296154));
#11802=CARTESIAN_POINT('Ctrl Pts',(2.00777602762851,6.34321180144366,2.87274675403155));
#11803=CARTESIAN_POINT('Ctrl Pts',(0.440583748475743,6.45423934201476,1.53892016467367));
#11804=CARTESIAN_POINT('Ctrl Pts',(-1.53193716163296,6.56526688258582,2.13609130675508));
#11805=CARTESIAN_POINT('Ctrl Pts',(-1.90934849916403,6.63928524296654,3.44784970607045));
#11806=CARTESIAN_POINT('Ctrl Pts',(-1.77928703864022,6.6762944231569,4.03891751659649));
#11807=CARTESIAN_POINT('Ctrl Pts',(-0.979727419285334,2.42387384126203,
2.27368025078364));
#11808=CARTESIAN_POINT('Ctrl Pts',(-1.43622363149362,2.46089489447305,2.59923419867212));
#11809=CARTESIAN_POINT('Ctrl Pts',(-1.99115683342641,2.53492512787443,3.73540524587877));
#11810=CARTESIAN_POINT('Ctrl Pts',(-1.00567667700427,2.64596454146616,5.37027542442224));
#11811=CARTESIAN_POINT('Ctrl Pts',(0.89946587290432,2.75699208203724,5.42597405909269));
#11812=CARTESIAN_POINT('Ctrl Pts',(1.98232364567101,2.86801962260832,3.85911121162473));
#11813=CARTESIAN_POINT('Ctrl Pts',(1.25429163898582,2.9790471631794,2.09756028172128));
#11814=CARTESIAN_POINT('Ctrl Pts',(-0.619853644373857,3.09007470375048,
1.75266217331931));
#11815=CARTESIAN_POINT('Ctrl Pts',(-1.9276020995976,3.20110224432155,3.13854330669838));
#11816=CARTESIAN_POINT('Ctrl Pts',(-1.47423759301864,3.31212978489263,4.98951092275774));
#11817=CARTESIAN_POINT('Ctrl Pts',(0.326079123896297,3.42315732546372,5.61416569991195));
#11818=CARTESIAN_POINT('Ctrl Pts',(1.82846474065272,3.53418486603478,4.44193237360281));
#11819=CARTESIAN_POINT('Ctrl Pts',(1.66028312568185,3.64521240660588,2.54374672152922));
#11820=CARTESIAN_POINT('Ctrl Pts',(-0.0248146850550805,3.75623994717694,
1.65391896491398));
#11821=CARTESIAN_POINT('Ctrl Pts',(-1.6872392535954,3.86726748774803,2.58541847779621));
#11822=CARTESIAN_POINT('Ctrl Pts',(-1.8081225654311,3.97829502831911,4.4871932051084));
#11823=CARTESIAN_POINT('Ctrl Pts',(-0.277018800711798,4.08932256889018,
5.6216860849489));
#11824=CARTESIAN_POINT('Ctrl Pts',(1.50718231204793,4.20035010946126,4.95237325924368));
#11825=CARTESIAN_POINT('Ctrl Pts',(1.91435013864119,4.31137765003234,3.09076929767337));
#11826=CARTESIAN_POINT('Ctrl Pts',(0.572476642613815,4.42240519060342,1.73772480837452));
#11827=CARTESIAN_POINT('Ctrl Pts',(-1.29243868422536,4.5334327311745,2.12944512822198));
#11828=CARTESIAN_POINT('Ctrl Pts',(-1.97652063896961,4.64446027174557,3.90803620554718));
#11829=CARTESIAN_POINT('Ctrl Pts',(-0.854759361360582,4.75548781231666,
5.44849250850354));
#11830=CARTESIAN_POINT('Ctrl Pts',(1.04795061858702,4.86651535288773,5.34338018015644));
#11831=CARTESIAN_POINT('Ctrl Pts',(1.99320324372482,4.97754289345882,3.68873447082252));
#11832=CARTESIAN_POINT('Ctrl Pts',(1.11737040425166,5.08857043402988,1.99631900565835));
#11833=CARTESIAN_POINT('Ctrl Pts',(-0.779344650934924,5.19959797460099,
1.81240372033652));
#11834=CARTESIAN_POINT('Ctrl Pts',(-1.96401433316682,5.31062551517205,3.305024781599));
#11835=CARTESIAN_POINT('Ctrl Pts',(-1.35426537751614,5.42165305574312,5.11044800058928));
#11836=CARTESIAN_POINT('Ctrl Pts',(0.492801319645515,5.53268059631421,5.5791618625879));
#11837=CARTESIAN_POINT('Ctrl Pts',(1.88962798045874,5.64370813688528,4.2829099175581));
#11838=CARTESIAN_POINT('Ctrl Pts',(1.55998788930993,5.75473567745637,2.40604260124246));
#11839=CARTESIAN_POINT('Ctrl Pts',(-0.194906614056223,5.86576321802745,
1.66329152996741));
#11840=CARTESIAN_POINT('Ctrl Pts',(-1.77177259431909,5.97679075859852,2.73339160557513));
#11841=CARTESIAN_POINT('Ctrl Pts',(-1.72977173752561,6.08781829916961,4.63841351254227));
#11842=CARTESIAN_POINT('Ctrl Pts',(-0.107544589451053,6.19884583974067,
5.63829066918126));
#11843=CARTESIAN_POINT('Ctrl Pts',(1.61327782397313,6.30987338031176,4.81861847686368));
#11844=CARTESIAN_POINT('Ctrl Pts',(1.85948240421865,6.42090092088282,2.92996195873161));
#11845=CARTESIAN_POINT('Ctrl Pts',(0.408042389490524,6.53192846145393,1.69465132693797));
#11846=CARTESIAN_POINT('Ctrl Pts',(-1.41878882765114,6.64295600202498,2.2477156208269));
#11847=CARTESIAN_POINT('Ctrl Pts',(-1.76832469800446,6.71697436240571,3.46258801124687));
#11848=CARTESIAN_POINT('Ctrl Pts',(-1.64786953070343,6.75398354259608,4.00999976347872));
#11849=CARTESIAN_POINT('Ctrl Pts',(-0.901594209403805,2.5015629607012,2.38323388698939));
#11850=CARTESIAN_POINT('Ctrl Pts',(-1.3216848728273,2.53858401391222,2.68282492474856));
#11851=CARTESIAN_POINT('Ctrl Pts',(-1.83236218124995,2.6126142473136,3.72838639101944));
#11852=CARTESIAN_POINT('Ctrl Pts',(-0.925474015191809,2.72365366090533,
5.23287575927349));
#11853=CARTESIAN_POINT('Ctrl Pts',(0.827733517102571,2.8346812014764,5.28413243077424));
#11854=CARTESIAN_POINT('Ctrl Pts',(1.82423343975097,2.94570874204748,3.84222681253854));
#11855=CARTESIAN_POINT('Ctrl Pts',(1.15426194710171,3.05673628261856,2.22115947614681));
#11856=CARTESIAN_POINT('Ctrl Pts',(-0.57042034901195,3.16776382318964,1.9037669736522));
#11857=CARTESIAN_POINT('Ctrl Pts',(-1.77387593408332,3.27879136376072,3.17912415992756));
#11858=CARTESIAN_POINT('Ctrl Pts',(-1.35666722293081,3.3898189043318,4.8824772064825));
#11859=CARTESIAN_POINT('Ctrl Pts',(0.30007433100813,3.50084644490287,5.45731579818944));
#11860=CARTESIAN_POINT('Ctrl Pts',(1.68264477427207,3.61187398547397,4.37856801766755));
#11861=CARTESIAN_POINT('Ctrl Pts',(1.52787563420194,3.72290152604503,2.6317625709737));
#11862=CARTESIAN_POINT('Ctrl Pts',(-0.0228357152341017,3.83392906661613,
1.81289853089582));
#11863=CARTESIAN_POINT('Ctrl Pts',(-1.55268201233978,3.94495660718718,2.67011100688194));
#11864=CARTESIAN_POINT('Ctrl Pts',(-1.66392488644871,4.05598414775829,4.42021930025391));
#11865=CARTESIAN_POINT('Ctrl Pts',(-0.254926566003359,4.16701168832935,
5.46423643291735));
#11866=CARTESIAN_POINT('Ctrl Pts',(1.38698460235958,4.27803922890044,4.84830126966989));
#11867=CARTESIAN_POINT('Ctrl Pts',(1.76168081631245,4.3890667694715,3.13516012559607));
#11868=CARTESIAN_POINT('Ctrl Pts',(0.526821660637044,4.5000943100426,1.8900208627719));
#11869=CARTESIAN_POINT('Ctrl Pts',(-1.18936676750056,4.61112185061366,2.25050150782511));
#11870=CARTESIAN_POINT('Ctrl Pts',(-1.81889322252715,4.72214939118475,3.88725004078275));
#11871=CARTESIAN_POINT('Ctrl Pts',(-0.786592347490432,4.83317693175582,
5.30485503503531));
#11872=CARTESIAN_POINT('Ctrl Pts',(0.964376612168716,4.9442044723269,5.2081254093157));
#11873=CARTESIAN_POINT('Ctrl Pts',(1.83424539043528,5.05523201289798,3.68543760780607));
#11874=CARTESIAN_POINT('Ctrl Pts',(1.02826017359741,5.16625955346907,2.12799218649641));
#11875=CARTESIAN_POINT('Ctrl Pts',(-0.717191956233407,5.27728709404013,
1.95874413545384));
#11876=CARTESIAN_POINT('Ctrl Pts',(-1.80738429395082,5.38831463461122,3.33232874600814));
#11877=CARTESIAN_POINT('Ctrl Pts',(-1.2462627852707,5.49934217518229,4.99376955875193));
#11878=CARTESIAN_POINT('Ctrl Pts',(0.453500440462359,5.61036971575338,5.42510351504104));
#11879=CARTESIAN_POINT('Ctrl Pts',(1.73893024893777,5.72139725632445,4.23222759408355));
#11880=CARTESIAN_POINT('Ctrl Pts',(1.43557893762722,5.83242479689554,2.50504034699825));
#11881=CARTESIAN_POINT('Ctrl Pts',(-0.179362821891601,5.9434523374666,1.82152363438183));
#11882=CARTESIAN_POINT('Ctrl Pts',(-1.63047382361075,6.0544798780377,2.80628328554509));
#11883=CARTESIAN_POINT('Ctrl Pts',(-1.59182253292561,6.16550741860876,4.55937979616623));
#11884=CARTESIAN_POINT('Ctrl Pts',(-0.0989679141291225,6.27653495917986,
5.47951680243522));
#11885=CARTESIAN_POINT('Ctrl Pts',(1.48461900281892,6.38756249975091,4.72521342411197));
#11886=CARTESIAN_POINT('Ctrl Pts',(1.71118878080877,6.49859004032201,2.98717716343168));
#11887=CARTESIAN_POINT('Ctrl Pts',(0.375501030505306,6.60961758089308,1.85038248920226));
#11888=CARTESIAN_POINT('Ctrl Pts',(-1.30564049366934,6.72064512146416,2.35933993489874));
#11889=CARTESIAN_POINT('Ctrl Pts',(-1.62730089684488,6.79466348184489,3.47732631642329));
#11890=CARTESIAN_POINT('Ctrl Pts',(-1.51645202276663,6.83167266203525,3.98108201036094));
#11891=CARTESIAN_POINT('Ctrl Pts',(0.426653165344753,6.6,2.14890699090199));
#11892=CARTESIAN_POINT('Ctrl Pts',(0.392021497824992,6.6,2.13398863376564));
#11893=CARTESIAN_POINT('Ctrl Pts',(0.356894299772026,6.6,2.12044962477061));
#11894=CARTESIAN_POINT('Ctrl Pts',(0.321336195052727,6.6,2.10833833927896));
#11895=CARTESIAN_POINT('Ctrl Pts',(0.265498001512556,6.6,2.08931954430544));
#11896=CARTESIAN_POINT('Ctrl Pts',(0.208598730014752,6.6,2.07381868408178));
#11897=CARTESIAN_POINT('Ctrl Pts',(0.1509393876911,6.6,2.06168379971155));
#11898=CARTESIAN_POINT('Ctrl Pts',(0.0913824050528511,6.6,2.04914954127866));
#11899=CARTESIAN_POINT('Ctrl Pts',(0.0310137753734779,6.6,2.04020620057528));
#11900=CARTESIAN_POINT('Ctrl Pts',(-0.0298636689844298,6.6,2.03473391296962));
#11901=CARTESIAN_POINT('Ctrl Pts',(-0.0578342380330448,6.6,2.03221963202464));
#11902=CARTESIAN_POINT('Ctrl Pts',(-0.0859125425645439,6.60000000000001,
2.03043876497219));
#11903=CARTESIAN_POINT('Ctrl Pts',(-0.114070466778639,6.60000000000001,
2.02938311428739));
#11904=CARTESIAN_POINT('Ctrl Pts',(-0.127825777649119,6.60000000000001,
2.02886742274601));
#11905=CARTESIAN_POINT('Ctrl Pts',(-0.14160009738174,6.6,2.02852482806012));
#11906=CARTESIAN_POINT('Ctrl Pts',(-0.155390186243194,6.6,2.02835456195388));
#11907=CARTESIAN_POINT('Ctrl Pts',(-0.168292536222095,6.6,2.02819525675183));
#11908=CARTESIAN_POINT('Ctrl Pts',(-0.181210508050245,6.6,2.02818695541747));
#11909=CARTESIAN_POINT('Ctrl Pts',(-0.194119545885251,6.6,2.02832850350773));
#11910=CARTESIAN_POINT('Ctrl Pts',(-0.257354814991631,6.6,2.02902188063574));
#11911=CARTESIAN_POINT('Ctrl Pts',(-0.320489102810685,6.6,2.03330438410903));
#11912=CARTESIAN_POINT('Ctrl Pts',(-0.383193278303246,6.6,2.04101811062465));
#11913=CARTESIAN_POINT('Ctrl Pts',(-0.447605187296912,6.6,2.0489419186713));
#11914=CARTESIAN_POINT('Ctrl Pts',(-0.511564220105741,6.6,2.06048621346354));
#11915=CARTESIAN_POINT('Ctrl Pts',(-0.574732782053451,6.6,2.07553202136673));
#11916=CARTESIAN_POINT('Ctrl Pts',(-0.63649384373375,6.6,2.09024258373015));
#11917=CARTESIAN_POINT('Ctrl Pts',(-0.69750033846162,6.6,2.10830059514023));
#11918=CARTESIAN_POINT('Ctrl Pts',(-0.757439278427627,6.6,2.12964296447379));
#11919=CARTESIAN_POINT('Ctrl Pts',(-0.770258979238349,6.6,2.13420765630189));
#11920=CARTESIAN_POINT('Ctrl Pts',(-0.783029821639415,6.6,2.13892276037541));
#11921=CARTESIAN_POINT('Ctrl Pts',(-0.795748686884653,6.6,2.14378793828041));
#11922=CARTESIAN_POINT('Ctrl Pts',(-0.804987038335825,6.6,2.14732176165949));
#11923=CARTESIAN_POINT('Ctrl Pts',(-0.814196614102969,6.6,2.15093430558212));
#11924=CARTESIAN_POINT('Ctrl Pts',(-0.823367217132576,6.6,2.15462160038541));
#11925=CARTESIAN_POINT('Ctrl Pts',(-0.885585027870816,6.6,2.1796379934695));
#11926=CARTESIAN_POINT('Ctrl Pts',(-0.946123259636302,6.6,2.208134350996));
#11927=CARTESIAN_POINT('Ctrl Pts',(-1.00463249706853,6.6,2.23997375780666));
#11928=CARTESIAN_POINT('Ctrl Pts',(-1.06301708457837,6.6,2.27174533294216));
#11929=CARTESIAN_POINT('Ctrl Pts',(-1.11938248584106,6.6,2.3068458567018));
#11930=CARTESIAN_POINT('Ctrl Pts',(-1.17337908184492,6.6,2.34519025207806));
#11931=CARTESIAN_POINT('Ctrl Pts',(-1.2011248982945,6.6,2.36489328217099));
#11932=CARTESIAN_POINT('Ctrl Pts',(-1.22824511864328,6.6,2.38545362353557));
#11933=CARTESIAN_POINT('Ctrl Pts',(-1.25469050295844,6.6,2.40686481674483));
#11934=CARTESIAN_POINT('Ctrl Pts',(-1.28458305880662,6.6,2.43106697169013));
#11935=CARTESIAN_POINT('Ctrl Pts',(-1.31361349719727,6.6,2.45635617344964));
#11936=CARTESIAN_POINT('Ctrl Pts',(-1.34176728722323,6.6,2.48267337167381));
#11937=CARTESIAN_POINT('Ctrl Pts',(-1.3504346031965,6.6,2.49077528165927));
#11938=CARTESIAN_POINT('Ctrl Pts',(-1.35902006809447,6.6,2.49897589013228));
#11939=CARTESIAN_POINT('Ctrl Pts',(-1.36751921647731,6.6,2.50726969035999));
#11940=CARTESIAN_POINT('Ctrl Pts',(-1.41452515694303,6.6,2.55313991902021));
#11941=CARTESIAN_POINT('Ctrl Pts',(-1.45871734531156,6.59999999999999,2.60168402751855));
#11942=CARTESIAN_POINT('Ctrl Pts',(-1.50006762008885,6.6,2.65254463268113));
#11943=CARTESIAN_POINT('Ctrl Pts',(-1.54232945728785,6.6,2.70452645449005));
#11944=CARTESIAN_POINT('Ctrl Pts',(-1.58162322286118,6.6,2.75892858938386));
#11945=CARTESIAN_POINT('Ctrl Pts',(-1.61789321674135,6.6,2.81541824090764));
#11946=CARTESIAN_POINT('Ctrl Pts',(-1.65493748507655,6.6,2.87311380645206));
#11947=CARTESIAN_POINT('Ctrl Pts',(-1.68882811749007,6.6,2.93298765877334));
#11948=CARTESIAN_POINT('Ctrl Pts',(-1.71947060296554,6.6,2.99472594037275));
#11949=CARTESIAN_POINT('Ctrl Pts',(-1.72737084986519,6.6,3.01064330674259));
#11950=CARTESIAN_POINT('Ctrl Pts',(-1.73505498274876,6.6,3.02668477919227));
#11951=CARTESIAN_POINT('Ctrl Pts',(-1.74252093472838,6.6,3.04284531382503));
#11952=CARTESIAN_POINT('Ctrl Pts',(-1.74801629841351,6.6,3.05474038298642));
#11953=CARTESIAN_POINT('Ctrl Pts',(-1.75339345226814,6.6,3.06669996022911));
#11954=CARTESIAN_POINT('Ctrl Pts',(-1.75865150299272,6.6,3.07872207225469));
#11955=CARTESIAN_POINT('Ctrl Pts',(-1.76360055617396,6.6,3.09003768613558));
#11956=CARTESIAN_POINT('Ctrl Pts',(-1.76844015488379,6.6,3.10139971532666));
#11957=CARTESIAN_POINT('Ctrl Pts',(-1.7731695901327,6.6,3.11280520805519));
#11958=CARTESIAN_POINT('Ctrl Pts',(-1.80041932407603,6.6,3.17852058969964));
#11959=CARTESIAN_POINT('Ctrl Pts',(-1.82401955599936,6.6,3.24568623985345));
#11960=CARTESIAN_POINT('Ctrl Pts',(-1.84389319792571,6.6,3.31394437456818));
#11961=CARTESIAN_POINT('Ctrl Pts',(-1.86154775130874,6.6,3.37458081390891));
#11962=CARTESIAN_POINT('Ctrl Pts',(-1.87626122909509,6.6,3.43608043801735));
#11963=CARTESIAN_POINT('Ctrl Pts',(-1.88795171174053,6.6,3.49821270276066));
#11964=CARTESIAN_POINT('Ctrl Pts',(-1.89137817487387,6.6,3.51642357745171));
#11965=CARTESIAN_POINT('Ctrl Pts',(-1.89454475421827,6.6,3.53468889469712));
#11966=CARTESIAN_POINT('Ctrl Pts',(-1.89744890219664,6.6,3.55300305372269));
#11967=CARTESIAN_POINT('Ctrl Pts',(-1.89980101601846,6.6,3.56783597095006));
#11968=CARTESIAN_POINT('Ctrl Pts',(-1.90197972571919,6.6,3.58269332806818));
#11969=CARTESIAN_POINT('Ctrl Pts',(-1.90398341147039,6.6,3.597565901918));
#11970=CARTESIAN_POINT('Ctrl Pts',(-1.91367106629463,6.6,3.6694735659412));
#11971=CARTESIAN_POINT('Ctrl Pts',(-1.91927795233211,6.6,3.74177918256837));
#11972=CARTESIAN_POINT('Ctrl Pts',(-1.920702872003,6.6,3.81413426671844));
#11973=CARTESIAN_POINT('Ctrl Pts',(-1.92211579885034,6.6,3.88588037495561));
#11974=CARTESIAN_POINT('Ctrl Pts',(-1.91941728760775,6.6,3.95767611430931));
#11975=CARTESIAN_POINT('Ctrl Pts',(-1.91246071929416,6.6,4.02919789216754));
#11976=CARTESIAN_POINT('Ctrl Pts',(-1.91122396329351,6.6,4.04191321155429));
#11977=CARTESIAN_POINT('Ctrl Pts',(-1.90985249159563,6.6,4.05461989137107));
#11978=CARTESIAN_POINT('Ctrl Pts',(-1.90834530359594,6.6,4.06731613031539));
#11979=CARTESIAN_POINT('Ctrl Pts',(-0.863580915426621,2.5,5.40376507534353));
#11980=CARTESIAN_POINT('Ctrl Pts',(-0.903481800679317,2.5,5.37926660921982));
#11981=CARTESIAN_POINT('Ctrl Pts',(-0.942351921741605,2.5,5.35328747129858));
#11982=CARTESIAN_POINT('Ctrl Pts',(-0.98009997800088,2.5,5.32582783981609));
#11983=CARTESIAN_POINT('Ctrl Pts',(-1.03746171315656,2.5,5.28410033740505));
#11984=CARTESIAN_POINT('Ctrl Pts',(-1.09223449276709,2.5,5.23895557017225));
#11985=CARTESIAN_POINT('Ctrl Pts',(-1.14428247580057,2.5,5.19073503960552));
#11986=CARTESIAN_POINT('Ctrl Pts',(-1.19702062674331,2.5,5.14187509400626));
#11987=CARTESIAN_POINT('Ctrl Pts',(-1.2469617357595,2.5,5.08985623930448));
#11988=CARTESIAN_POINT('Ctrl Pts',(-1.2939195274248,2.5,5.03500604649739));
#11989=CARTESIAN_POINT('Ctrl Pts',(-1.31490326590717,2.5,5.01049547943804));
#11990=CARTESIAN_POINT('Ctrl Pts',(-1.33529063452927,2.5,4.98541925943203));
#11991=CARTESIAN_POINT('Ctrl Pts',(-1.35506176433983,2.5,4.95980570446106));
#11992=CARTESIAN_POINT('Ctrl Pts',(-1.36763974825088,2.5,4.94351089048651));
#11993=CARTESIAN_POINT('Ctrl Pts',(-1.37996828403753,2.5,4.92699859586587));
#11994=CARTESIAN_POINT('Ctrl Pts',(-1.39204180474552,2.5,4.91027607043345));
#11995=CARTESIAN_POINT('Ctrl Pts',(-1.39932292816931,2.5,4.90019129279686));
#11996=CARTESIAN_POINT('Ctrl Pts',(-1.40651184411551,2.5,4.89002911341411));
#11997=CARTESIAN_POINT('Ctrl Pts',(-1.41359773398804,2.5,4.87980534670441));
#11998=CARTESIAN_POINT('Ctrl Pts',(-1.45372898056346,2.5,4.82190259770073));
#11999=CARTESIAN_POINT('Ctrl Pts',(-1.49063491985867,2.5,4.76192357985326));
#12000=CARTESIAN_POINT('Ctrl Pts',(-1.52417445455585,2.5,4.70019324906169));
#12001=CARTESIAN_POINT('Ctrl Pts',(-1.55724799448755,2.5,4.63932059298981));
#12002=CARTESIAN_POINT('Ctrl Pts',(-1.58704824364224,2.5,4.57674389643576));
#12003=CARTESIAN_POINT('Ctrl Pts',(-1.61339223678792,2.5,4.51276105665826));
#12004=CARTESIAN_POINT('Ctrl Pts',(-1.6391925849168,2.5,4.45009859195879));
#12005=CARTESIAN_POINT('Ctrl Pts',(-1.66167798028648,2.5,4.38608652284999));
#12006=CARTESIAN_POINT('Ctrl Pts',(-1.68062808015966,2.5,4.32100573109058));
#12007=CARTESIAN_POINT('Ctrl Pts',(-1.68520397395377,2.5,4.30529062704781));
#12008=CARTESIAN_POINT('Ctrl Pts',(-1.6895735006115,2.5,4.28951324694272));
#12009=CARTESIAN_POINT('Ctrl Pts',(-1.69373310940874,2.5,4.27367764319859));
#12010=CARTESIAN_POINT('Ctrl Pts',(-1.69762827691426,2.5,4.25884876573892));
#12011=CARTESIAN_POINT('Ctrl Pts',(-1.70134027319327,2.5,4.24396443862568));
#12012=CARTESIAN_POINT('Ctrl Pts',(-1.70485982263115,2.5,4.22905603380731));
#12013=CARTESIAN_POINT('Ctrl Pts',(-1.72026850374742,2.5,4.16378664070643));
#12014=CARTESIAN_POINT('Ctrl Pts',(-1.73201964293625,2.5,4.09796147517623));
#12015=CARTESIAN_POINT('Ctrl Pts',(-1.73995104778309,2.5,4.03185909019967));
#12016=CARTESIAN_POINT('Ctrl Pts',(-1.74764478811313,2.5,3.9677374629435));
#12017=CARTESIAN_POINT('Ctrl Pts',(-1.751744263924,2.5,3.9033541748481));
#12018=CARTESIAN_POINT('Ctrl Pts',(-1.75205333162731,2.5,3.83896894622793));
#12019=CARTESIAN_POINT('Ctrl Pts',(-1.7522329238389,2.5,3.80155615453879));
#12020=CARTESIAN_POINT('Ctrl Pts',(-1.75113178109468,2.5,3.76414287275013));
#12021=CARTESIAN_POINT('Ctrl Pts',(-1.74870362584431,2.5,3.72678250885966));
#12022=CARTESIAN_POINT('Ctrl Pts',(-1.74647840079727,2.5,3.69254449319611));
#12023=CARTESIAN_POINT('Ctrl Pts',(-1.74313852381005,2.5,3.65835091190104));
#12024=CARTESIAN_POINT('Ctrl Pts',(-1.73870317030217,2.5,3.62424537115788));
#12025=CARTESIAN_POINT('Ctrl Pts',(-1.73685252518326,2.5,3.61001488143665));
#12026=CARTESIAN_POINT('Ctrl Pts',(-1.73481112807366,2.5,3.59579974532177));
#12027=CARTESIAN_POINT('Ctrl Pts',(-1.73258023476447,2.5,3.5816032511338));
#12028=CARTESIAN_POINT('Ctrl Pts',(-1.73102147713403,2.5,3.57168395398501));
#12029=CARTESIAN_POINT('Ctrl Pts',(-1.72937055372535,2.5,3.56177631077978));
#12030=CARTESIAN_POINT('Ctrl Pts',(-1.72762964037198,2.5,3.55188979170823));
#12031=CARTESIAN_POINT('Ctrl Pts',(-1.71638514771449,2.5,3.48803314376386));
#12032=CARTESIAN_POINT('Ctrl Pts',(-1.70137472204148,2.5,3.42495366737195));
#12033=CARTESIAN_POINT('Ctrl Pts',(-1.68279990506686,2.5,3.36291988638466));
#12034=CARTESIAN_POINT('Ctrl Pts',(-1.6640678406117,2.5,3.30036095051798));
#12035=CARTESIAN_POINT('Ctrl Pts',(-1.64171010531439,2.5,3.23886455924878));
#12036=CARTESIAN_POINT('Ctrl Pts',(-1.61588779042438,2.5,3.17873192052349));
#12037=CARTESIAN_POINT('Ctrl Pts',(-1.59790265814149,2.5,3.13684979389774));
#12038=CARTESIAN_POINT('Ctrl Pts',(-1.57823587689003,2.5,3.09562976391068));
#12039=CARTESIAN_POINT('Ctrl Pts',(-1.55693161087442,2.5,3.05518450517549));
#12040=CARTESIAN_POINT('Ctrl Pts',(-1.54404063803802,2.5,3.03071153195339));
#12041=CARTESIAN_POINT('Ctrl Pts',(-1.53054997830694,2.5,3.00652241595214));
#12042=CARTESIAN_POINT('Ctrl Pts',(-1.51646823518921,2.5,2.98264409713377));
#12043=CARTESIAN_POINT('Ctrl Pts',(-1.50751920801676,2.5,2.9674692908508));
#12044=CARTESIAN_POINT('Ctrl Pts',(-1.49832995810422,2.5,2.95241815434546));
#12045=CARTESIAN_POINT('Ctrl Pts',(-1.48892012002058,2.5,2.93752436847607));
#12046=CARTESIAN_POINT('Ctrl Pts',(-1.45509045248929,2.5,2.88397915125075));
#12047=CARTESIAN_POINT('Ctrl Pts',(-1.41836558695713,2.5,2.83238306268947));
#12048=CARTESIAN_POINT('Ctrl Pts',(-1.37888773636291,2.5,2.78302628084676));
#12049=CARTESIAN_POINT('Ctrl Pts',(-1.34707041524265,2.5,2.74324699819296));
#12050=CARTESIAN_POINT('Ctrl Pts',(-1.31346403250493,2.5,2.70492277456948));
#12051=CARTESIAN_POINT('Ctrl Pts',(-1.2781304993022,2.5,2.6682268367928));
#12052=CARTESIAN_POINT('Ctrl Pts',(-1.26549763847924,2.5,2.65510687304502));
#12053=CARTESIAN_POINT('Ctrl Pts',(-1.25264391285156,2.5,2.64219524938621));
#12054=CARTESIAN_POINT('Ctrl Pts',(-1.23957189875077,2.5,2.62950057751442));
#12055=CARTESIAN_POINT('Ctrl Pts',(-1.23011804990801,2.5,2.6203196274283));
#12056=CARTESIAN_POINT('Ctrl Pts',(-1.22055629637473,2.5,2.61125828180734));
#12057=CARTESIAN_POINT('Ctrl Pts',(-1.21089009783154,2.5,2.60232128125257));
#12058=CARTESIAN_POINT('Ctrl Pts',(-1.16593824479678,2.5,2.56076050286437));
#12059=CARTESIAN_POINT('Ctrl Pts',(-1.11871429572448,2.5,2.52187040319554));
#12060=CARTESIAN_POINT('Ctrl Pts',(-1.06933638089194,2.5,2.48594621693763));
#12061=CARTESIAN_POINT('Ctrl Pts',(-1.01995846605941,2.5,2.45002203067972));
#12062=CARTESIAN_POINT('Ctrl Pts',(-0.968425945006883,2.5,2.417063104816));
#12063=CARTESIAN_POINT('Ctrl Pts',(-0.914840821515225,2.5,2.38741840352973));
#12064=CARTESIAN_POINT('Ctrl Pts',(-0.911106104638903,2.5,2.38535225981347));
#12065=CARTESIAN_POINT('Ctrl Pts',(-0.907361412730045,2.5,2.38330223944491));
#12066=CARTESIAN_POINT('Ctrl Pts',(-0.903606778650209,2.5,2.38126847156104));
#12067=CARTESIAN_POINT('Origin',(-1.46549439250521E-15,6.6,3.64739446828387));
#12068=CARTESIAN_POINT('',(1.15470053837925,6.6,3.64739446828387));
#12069=CARTESIAN_POINT('',(0.577350269189624,6.6,4.64739446828387));
#12070=CARTESIAN_POINT('',(1.01036297108184,6.6,3.89739446828387));
#12071=CARTESIAN_POINT('',(-0.577350269189628,6.6,4.64739446828387));
#12072=CARTESIAN_POINT('',(0.288675134594811,6.6,4.64739446828387));
#12073=CARTESIAN_POINT('',(-1.15470053837925,6.6,3.64739446828387));
#12074=CARTESIAN_POINT('',(-0.721687836487034,6.6,4.39739446828387));
#12075=CARTESIAN_POINT('',(-0.577350269189627,6.6,2.64739446828387));
#12076=CARTESIAN_POINT('',(-1.01036297108185,6.6,3.39739446828387));
#12077=CARTESIAN_POINT('',(0.577350269189625,6.6,2.64739446828387));
#12078=CARTESIAN_POINT('',(-0.288675134594814,6.6,2.64739446828387));
#12079=CARTESIAN_POINT('',(0.721687836487031,6.6,2.89739446828387));
#12080=CARTESIAN_POINT('Origin',(1.15470053837925,6.6,3.64739446828387));
#12081=CARTESIAN_POINT('',(1.15470053837925,6.1,3.64739446828387));
#12082=CARTESIAN_POINT('',(1.15470053837925,6.6,3.64739446828387));
#12083=CARTESIAN_POINT('',(0.577350269189624,6.1,4.64739446828387));
#12084=CARTESIAN_POINT('',(0.577350269189624,6.1,4.64739446828387));
#12085=CARTESIAN_POINT('',(0.577350269189624,6.6,4.64739446828387));
#12086=CARTESIAN_POINT('Origin',(0.577350269189625,6.6,2.64739446828387));
#12087=CARTESIAN_POINT('',(0.577350269189625,6.1,2.64739446828387));
#12088=CARTESIAN_POINT('',(0.577350269189625,6.6,2.64739446828387));
#12089=CARTESIAN_POINT('',(1.15470053837925,6.1,3.64739446828387));
#12090=CARTESIAN_POINT('Origin',(-0.577350269189627,6.6,2.64739446828387));
#12091=CARTESIAN_POINT('',(-0.577350269189626,6.1,2.64739446828387));
#12092=CARTESIAN_POINT('',(-0.577350269189627,6.6,2.64739446828387));
#12093=CARTESIAN_POINT('',(0.577350269189625,6.1,2.64739446828387));
#12094=CARTESIAN_POINT('Origin',(-1.15470053837925,6.6,3.64739446828387));
#12095=CARTESIAN_POINT('',(-1.15470053837925,6.1,3.64739446828387));
#12096=CARTESIAN_POINT('',(-1.15470053837925,6.6,3.64739446828387));
#12097=CARTESIAN_POINT('',(-0.577350269189626,6.1,2.64739446828387));
#12098=CARTESIAN_POINT('Origin',(-0.577350269189628,6.6,4.64739446828387));
#12099=CARTESIAN_POINT('',(-0.577350269189628,6.1,4.64739446828387));
#12100=CARTESIAN_POINT('',(-0.577350269189628,6.6,4.64739446828387));
#12101=CARTESIAN_POINT('',(-1.15470053837925,6.1,3.64739446828387));
#12102=CARTESIAN_POINT('Origin',(0.577350269189624,6.6,4.64739446828387));
#12103=CARTESIAN_POINT('',(-0.577350269189628,6.1,4.64739446828387));
#12104=CARTESIAN_POINT('Origin',(-1.35447209004269E-15,6.1,3.64739446828387));
#12105=CARTESIAN_POINT('Origin',(-5.55111512312578E-16,2.5,3.64739446828387));
#12106=CARTESIAN_POINT('',(0.,0.,0.));
#12107=CARTESIAN_POINT('',(0.,0.,0.));
#12108=CARTESIAN_POINT('',(0.,0.,0.));
#12109=UNCERTAINTY_MEASURE_WITH_UNIT(LENGTH_MEASURE(0.01),#12119,
'DISTANCE_ACCURACY_VALUE',
'Maximum model space distance between geometric entities at asserted c
onnectivities');
#12110=UNCERTAINTY_MEASURE_WITH_UNIT(LENGTH_MEASURE(0.01),#12119,
'DISTANCE_ACCURACY_VALUE',
'Maximum model space distance between geometric entities at asserted c
onnectivities');
#12111=UNCERTAINTY_MEASURE_WITH_UNIT(LENGTH_MEASURE(0.01),#12119,
'DISTANCE_ACCURACY_VALUE',
'Maximum model space distance between geometric entities at asserted c
onnectivities');
#12112=UNCERTAINTY_MEASURE_WITH_UNIT(LENGTH_MEASURE(0.01),#12119,
'DISTANCE_ACCURACY_VALUE',
'Maximum model space distance between geometric entities at asserted c
onnectivities');
#12113=UNCERTAINTY_MEASURE_WITH_UNIT(LENGTH_MEASURE(0.01),#12119,
'DISTANCE_ACCURACY_VALUE',
'Maximum model space distance between geometric entities at asserted c
onnectivities');
#12114=(
GEOMETRIC_REPRESENTATION_CONTEXT(3)
GLOBAL_UNCERTAINTY_ASSIGNED_CONTEXT((#12109))
GLOBAL_UNIT_ASSIGNED_CONTEXT((#12119,#12121,#12122))
REPRESENTATION_CONTEXT('','3D')
);
#12115=(
GEOMETRIC_REPRESENTATION_CONTEXT(3)
GLOBAL_UNCERTAINTY_ASSIGNED_CONTEXT((#12110))
GLOBAL_UNIT_ASSIGNED_CONTEXT((#12119,#12121,#12122))
REPRESENTATION_CONTEXT('','3D')
);
#12116=(
GEOMETRIC_REPRESENTATION_CONTEXT(3)
GLOBAL_UNCERTAINTY_ASSIGNED_CONTEXT((#12111))
GLOBAL_UNIT_ASSIGNED_CONTEXT((#12119,#12121,#12122))
REPRESENTATION_CONTEXT('','3D')
);
#12117=(
GEOMETRIC_REPRESENTATION_CONTEXT(3)
GLOBAL_UNCERTAINTY_ASSIGNED_CONTEXT((#12112))
GLOBAL_UNIT_ASSIGNED_CONTEXT((#12119,#12121,#12122))
REPRESENTATION_CONTEXT('','3D')
);
#12118=(
GEOMETRIC_REPRESENTATION_CONTEXT(3)
GLOBAL_UNCERTAINTY_ASSIGNED_CONTEXT((#12113))
GLOBAL_UNIT_ASSIGNED_CONTEXT((#12119,#12121,#12122))
REPRESENTATION_CONTEXT('','3D')
);
#12119=(
LENGTH_UNIT()
NAMED_UNIT(*)
SI_UNIT(.MILLI.,.METRE.)
);
#12120=(
LENGTH_UNIT()
NAMED_UNIT(*)
SI_UNIT($,.METRE.)
);
#12121=(
NAMED_UNIT(*)
PLANE_ANGLE_UNIT()
SI_UNIT($,.RADIAN.)
);
#12122=(
NAMED_UNIT(*)
SI_UNIT($,.STERADIAN.)
SOLID_ANGLE_UNIT()
);
#12123=SHAPE_DEFINITION_REPRESENTATION(#12127,#12134);
#12124=SHAPE_DEFINITION_REPRESENTATION(#12128,#12135);
#12125=SHAPE_DEFINITION_REPRESENTATION(#12129,#12136);
#12126=SHAPE_DEFINITION_REPRESENTATION(#12130,#12137);
#12127=PRODUCT_DEFINITION_SHAPE('',$,#12139);
#12128=PRODUCT_DEFINITION_SHAPE('',$,#12140);
#12129=PRODUCT_DEFINITION_SHAPE('',$,#12141);
#12130=PRODUCT_DEFINITION_SHAPE('',$,#12142);
#12131=PRODUCT_DEFINITION_SHAPE($,$,#20);
#12132=PRODUCT_DEFINITION_SHAPE($,$,#21);
#12133=PRODUCT_DEFINITION_SHAPE($,$,#22);
#12134=SHAPE_REPRESENTATION('',(#2443,#2723,#2724,#2725),#12114);
#12135=SHAPE_REPRESENTATION('',(#2444),#12115);
#12136=SHAPE_REPRESENTATION('',(#2667),#12116);
#12137=SHAPE_REPRESENTATION('',(#2695),#12117);
#12138=PRODUCT_DEFINITION_CONTEXT('part definition',#12152,'design');
#12139=PRODUCT_DEFINITION('BR-253','BR-253',#12143,#12138);
#12140=PRODUCT_DEFINITION('Pully','Pully',#12144,#12138);
#12141=PRODUCT_DEFINITION('Screw_01','Screw_01',#12145,#12138);
#12142=PRODUCT_DEFINITION('Screw_02','Screw_02',#12146,#12138);
#12143=PRODUCT_DEFINITION_FORMATION('',$,#12154);
#12144=PRODUCT_DEFINITION_FORMATION('',$,#12155);
#12145=PRODUCT_DEFINITION_FORMATION('',$,#12156);
#12146=PRODUCT_DEFINITION_FORMATION('',$,#12157);
#12147=PRODUCT_RELATED_PRODUCT_CATEGORY('BR-253','BR-253',(#12154));
#12148=PRODUCT_RELATED_PRODUCT_CATEGORY('Pully','Pully',(#12155));
#12149=PRODUCT_RELATED_PRODUCT_CATEGORY('Screw_01','Screw_01',(#12156));
#12150=PRODUCT_RELATED_PRODUCT_CATEGORY('Screw_02','Screw_02',(#12157));
#12151=APPLICATION_PROTOCOL_DEFINITION('international standard',
'automotive_design',2009,#12152);
#12152=APPLICATION_CONTEXT(
'Core Data for Automotive Mechanical Design Process');
#12153=PRODUCT_CONTEXT('part definition',#12152,'mechanical');
#12154=PRODUCT('BR-253','BR-253',$,(#12153));
#12155=PRODUCT('Pully','Pully',$,(#12153));
#12156=PRODUCT('Screw_01','Screw_01',$,(#12153));
#12157=PRODUCT('Screw_02','Screw_02',$,(#12153));
#12158=PRESENTATION_STYLE_ASSIGNMENT((#12160));
#12159=PRESENTATION_STYLE_ASSIGNMENT((#12161));
#12160=SURFACE_STYLE_USAGE(.BOTH.,#12162);
#12161=SURFACE_STYLE_USAGE(.BOTH.,#12163);
#12162=SURFACE_SIDE_STYLE('',(#12164));
#12163=SURFACE_SIDE_STYLE('',(#12165));
#12164=SURFACE_STYLE_FILL_AREA(#12166);
#12165=SURFACE_STYLE_FILL_AREA(#12167);
#12166=FILL_AREA_STYLE('Steel - Satin',(#12168));
#12167=FILL_AREA_STYLE('Opaque(160,160,160)',(#12169));
#12168=FILL_AREA_STYLE_COLOUR('Steel - Satin',#12170);
#12169=FILL_AREA_STYLE_COLOUR('Opaque(160,160,160)',#12171);
#12170=COLOUR_RGB('Steel - Satin', 0.09019608, 0.27058824, 0.51372549);
#12171=COLOUR_RGB('Opaque(160,160,160)', 0.09019608, 0.27058824, 0.51372549);
ENDSEC;
END-ISO-10303-21;
